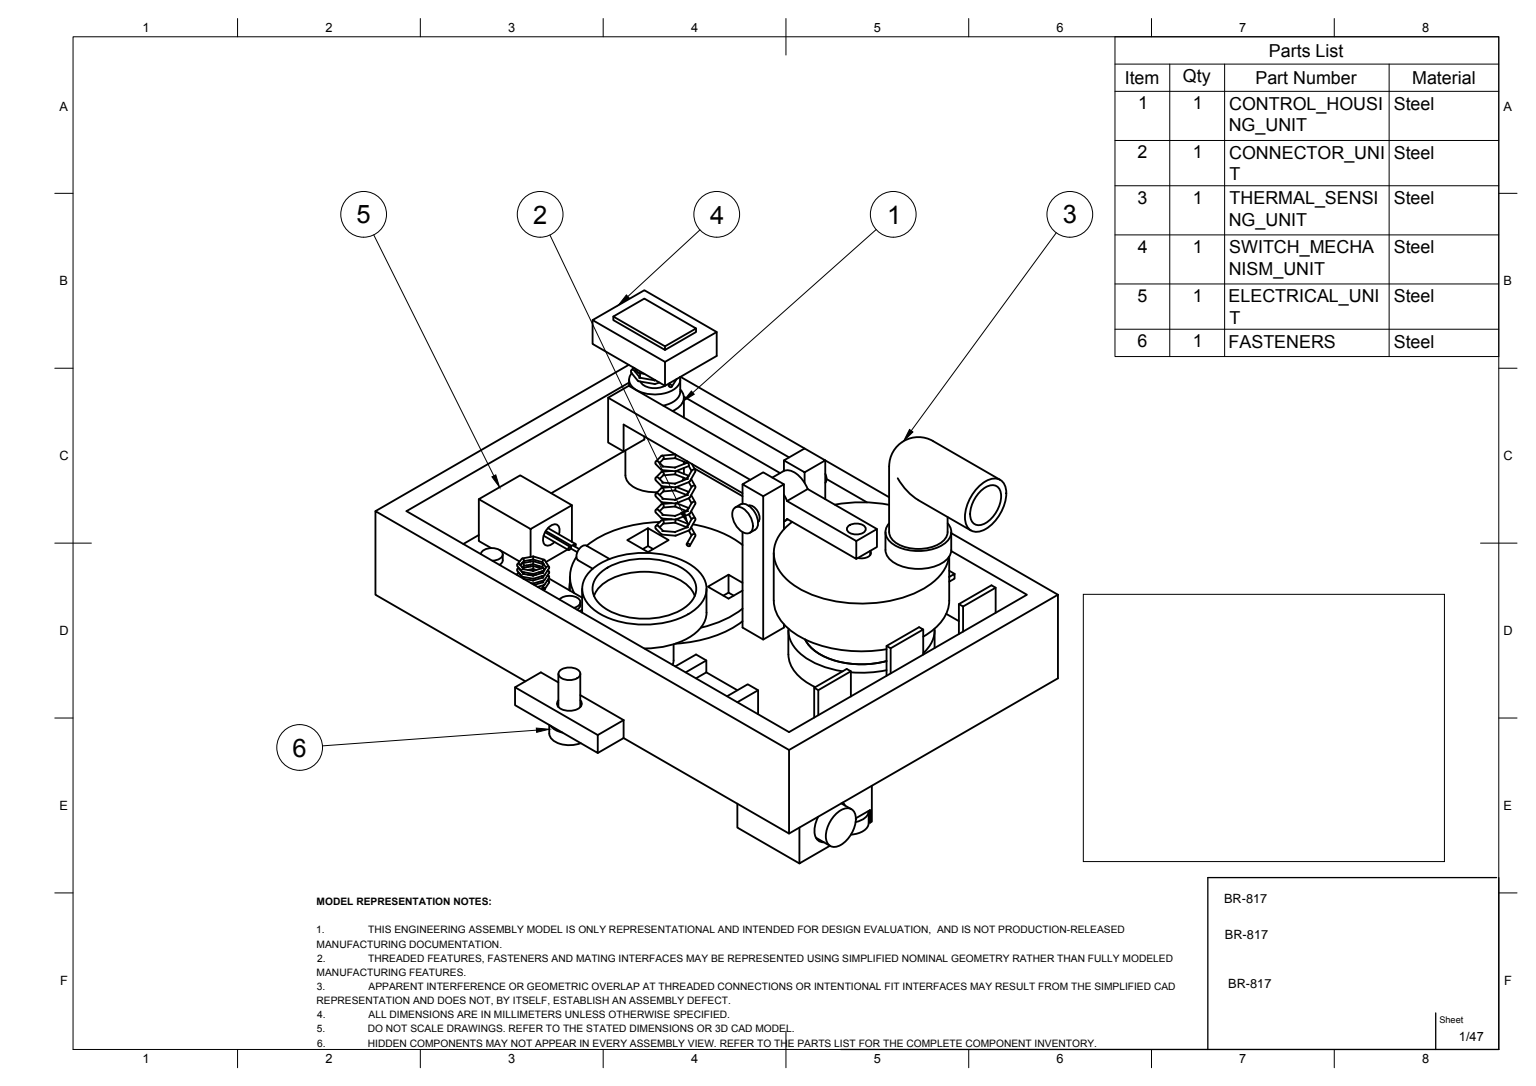
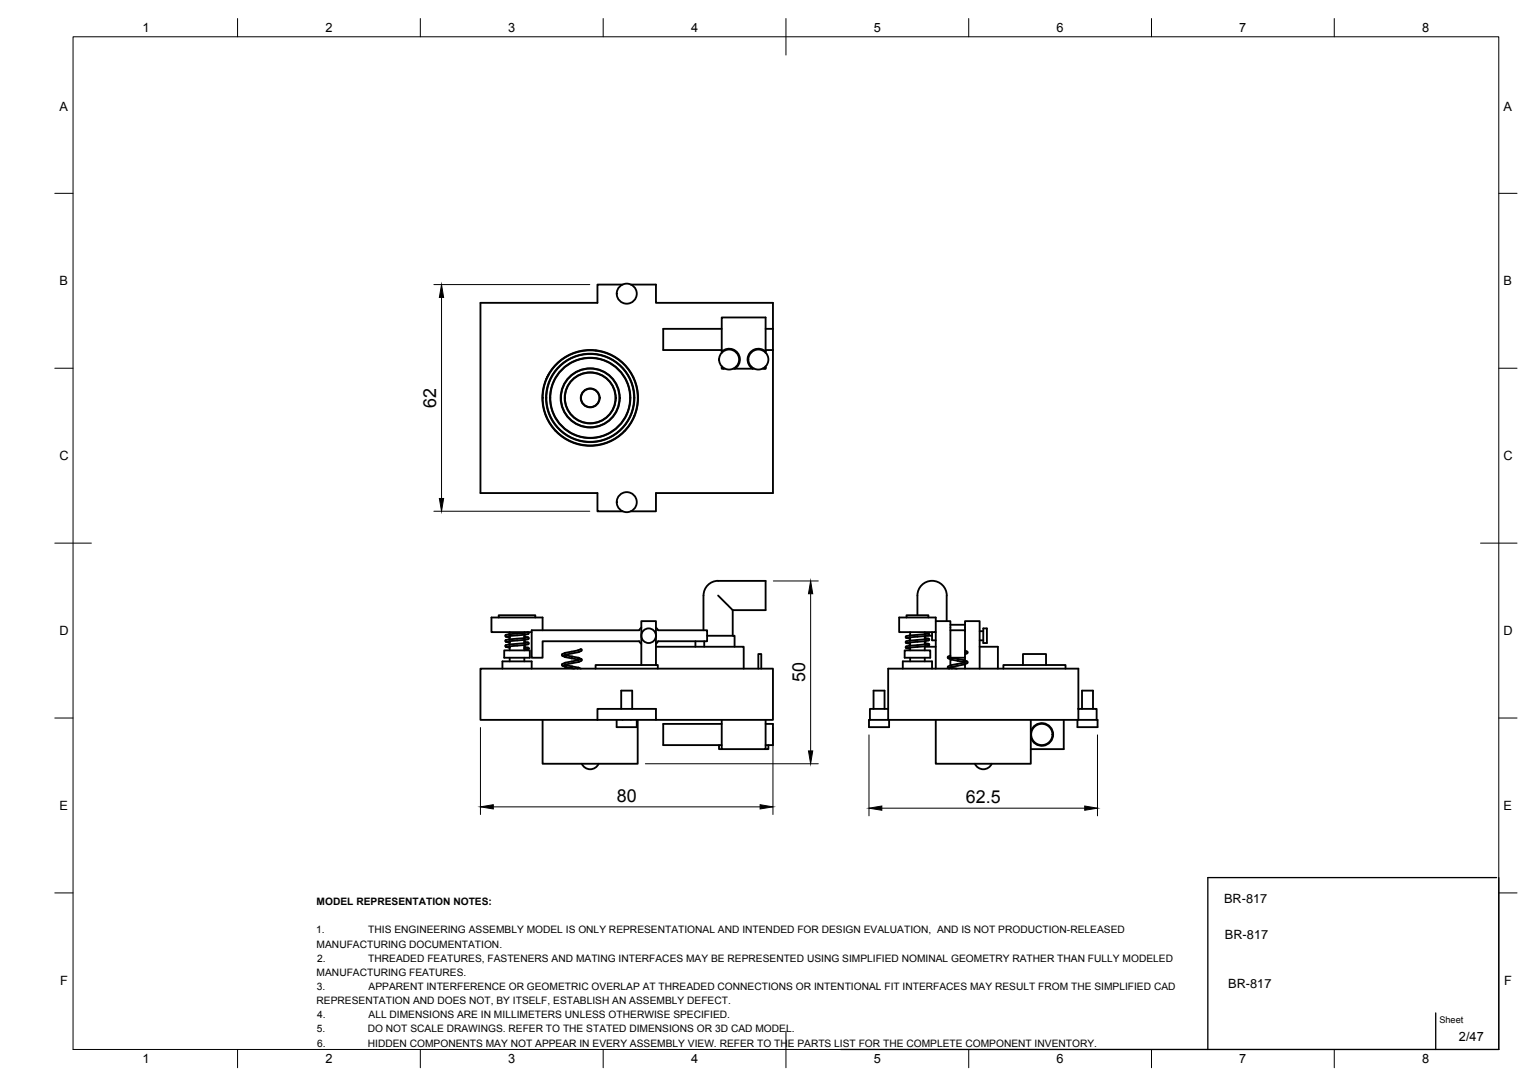
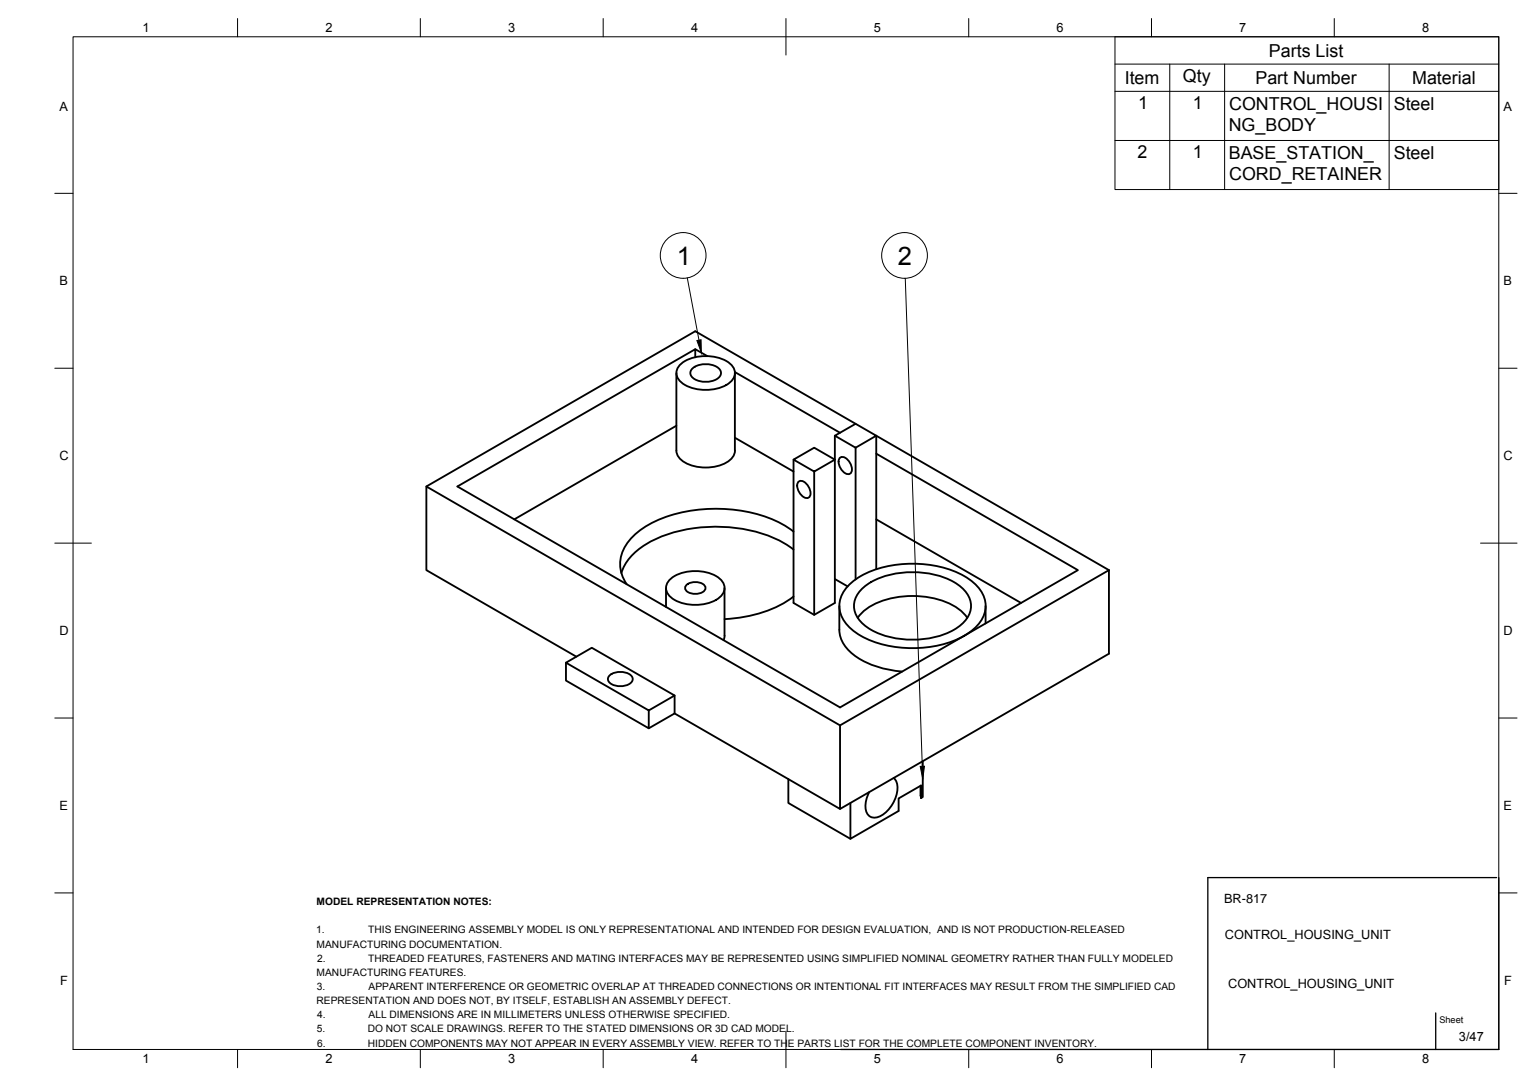
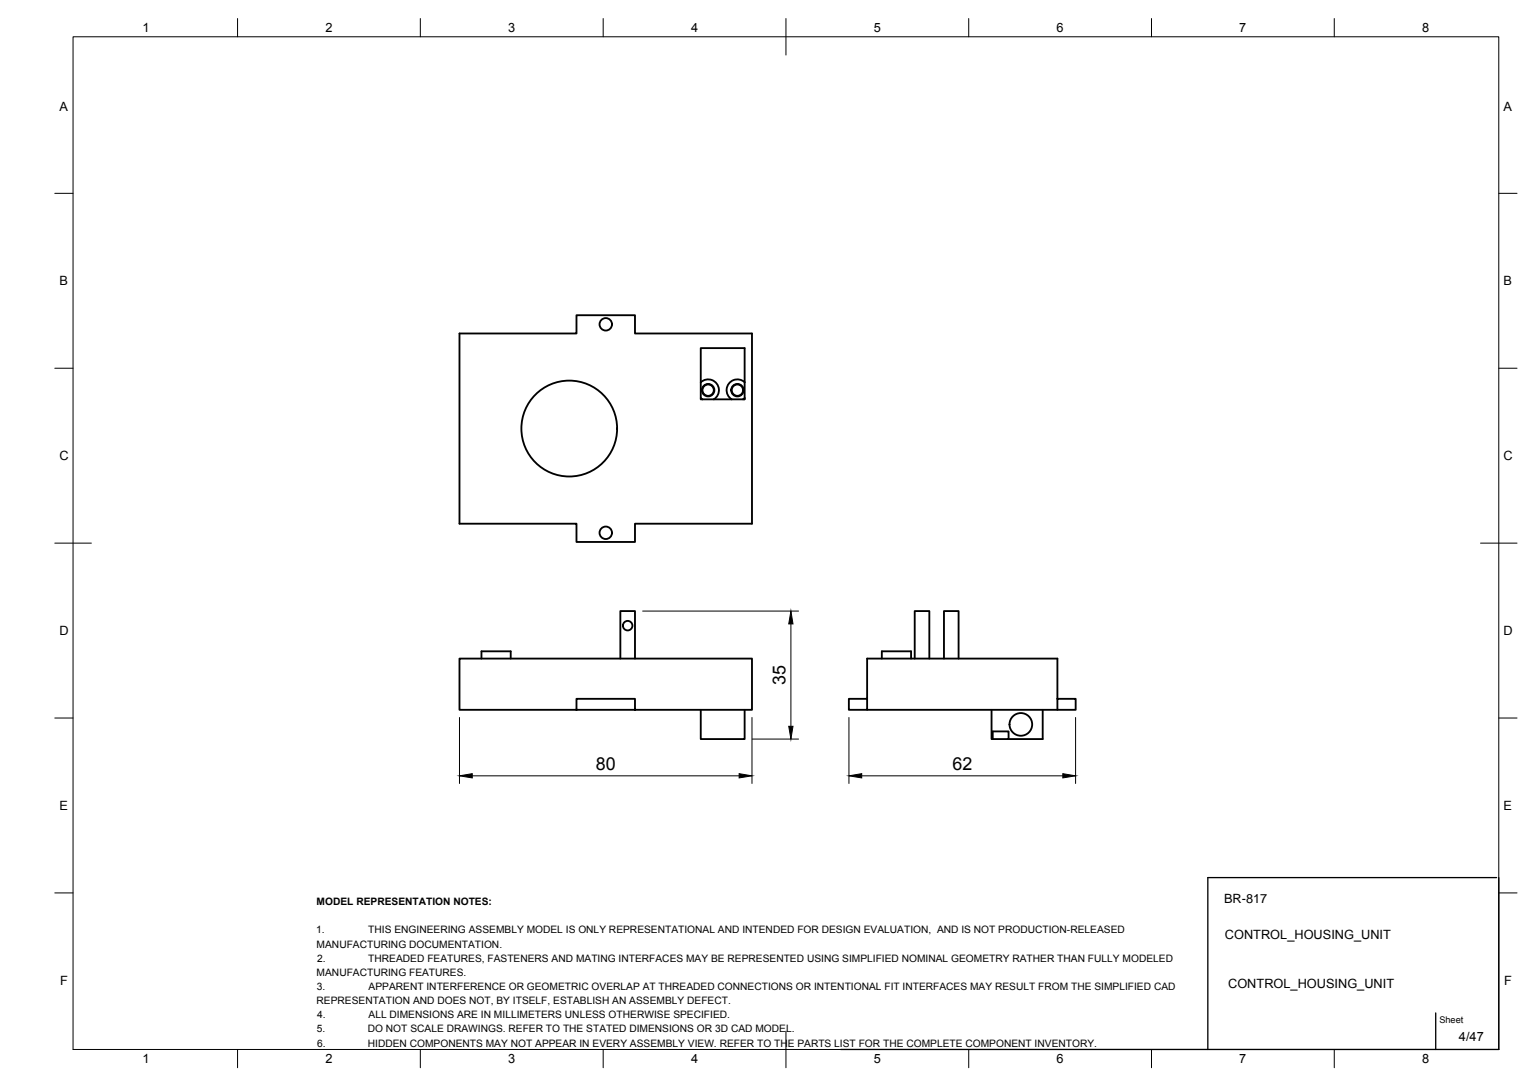
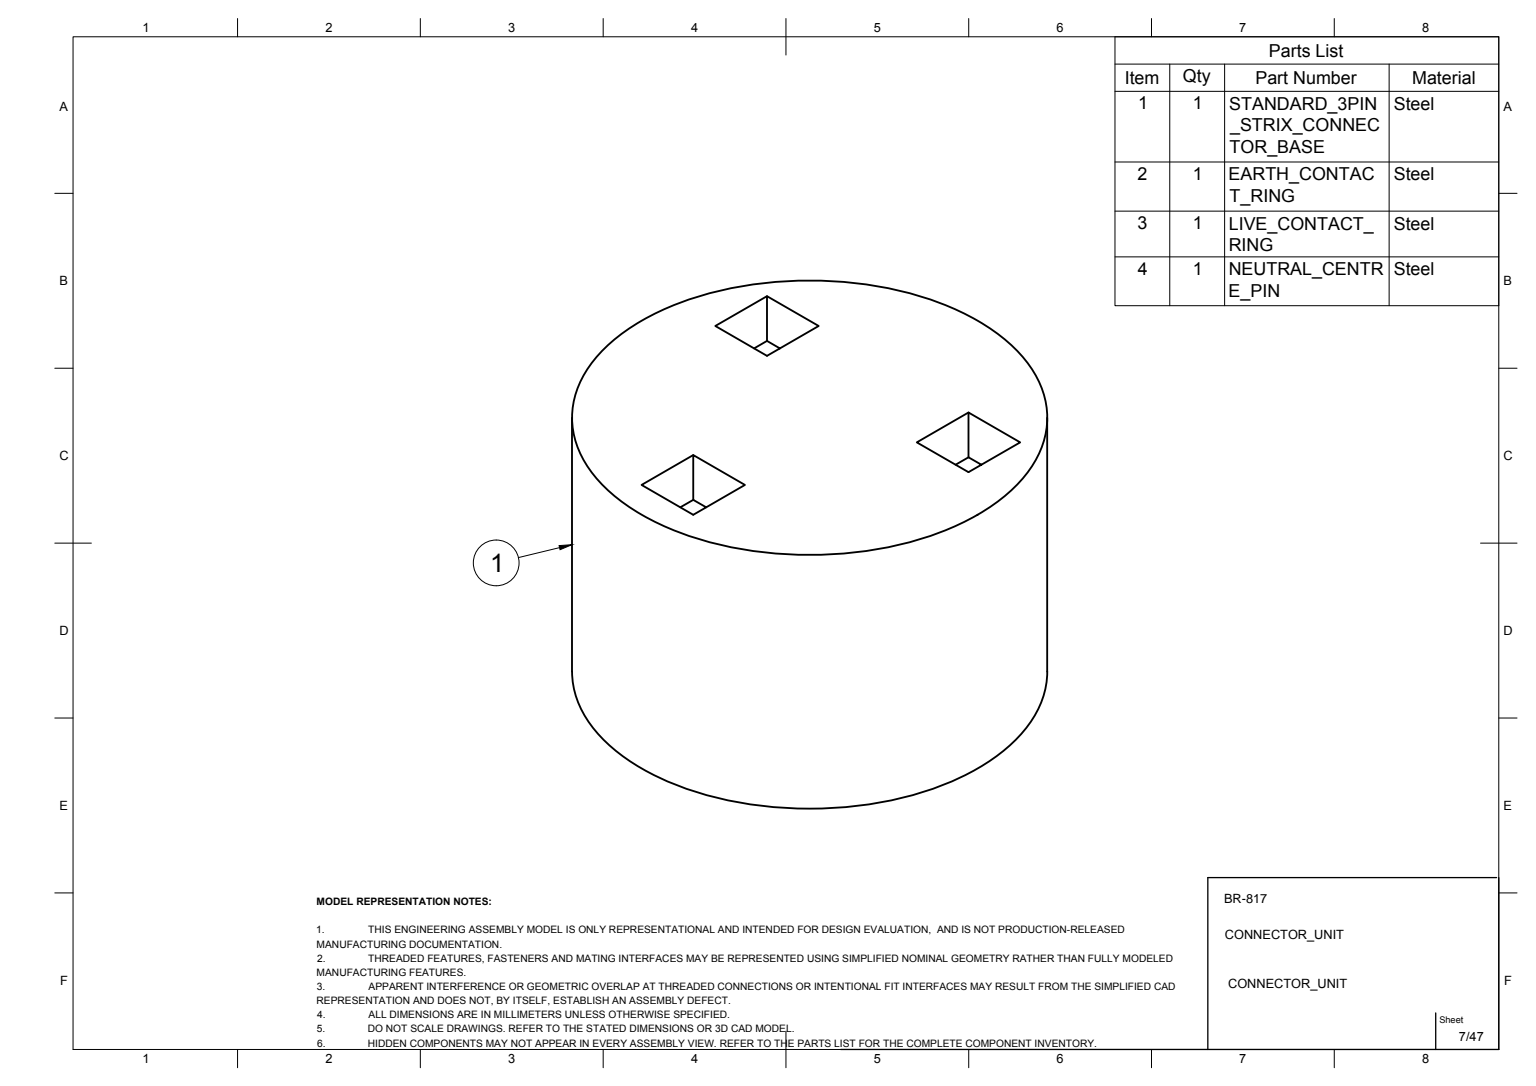
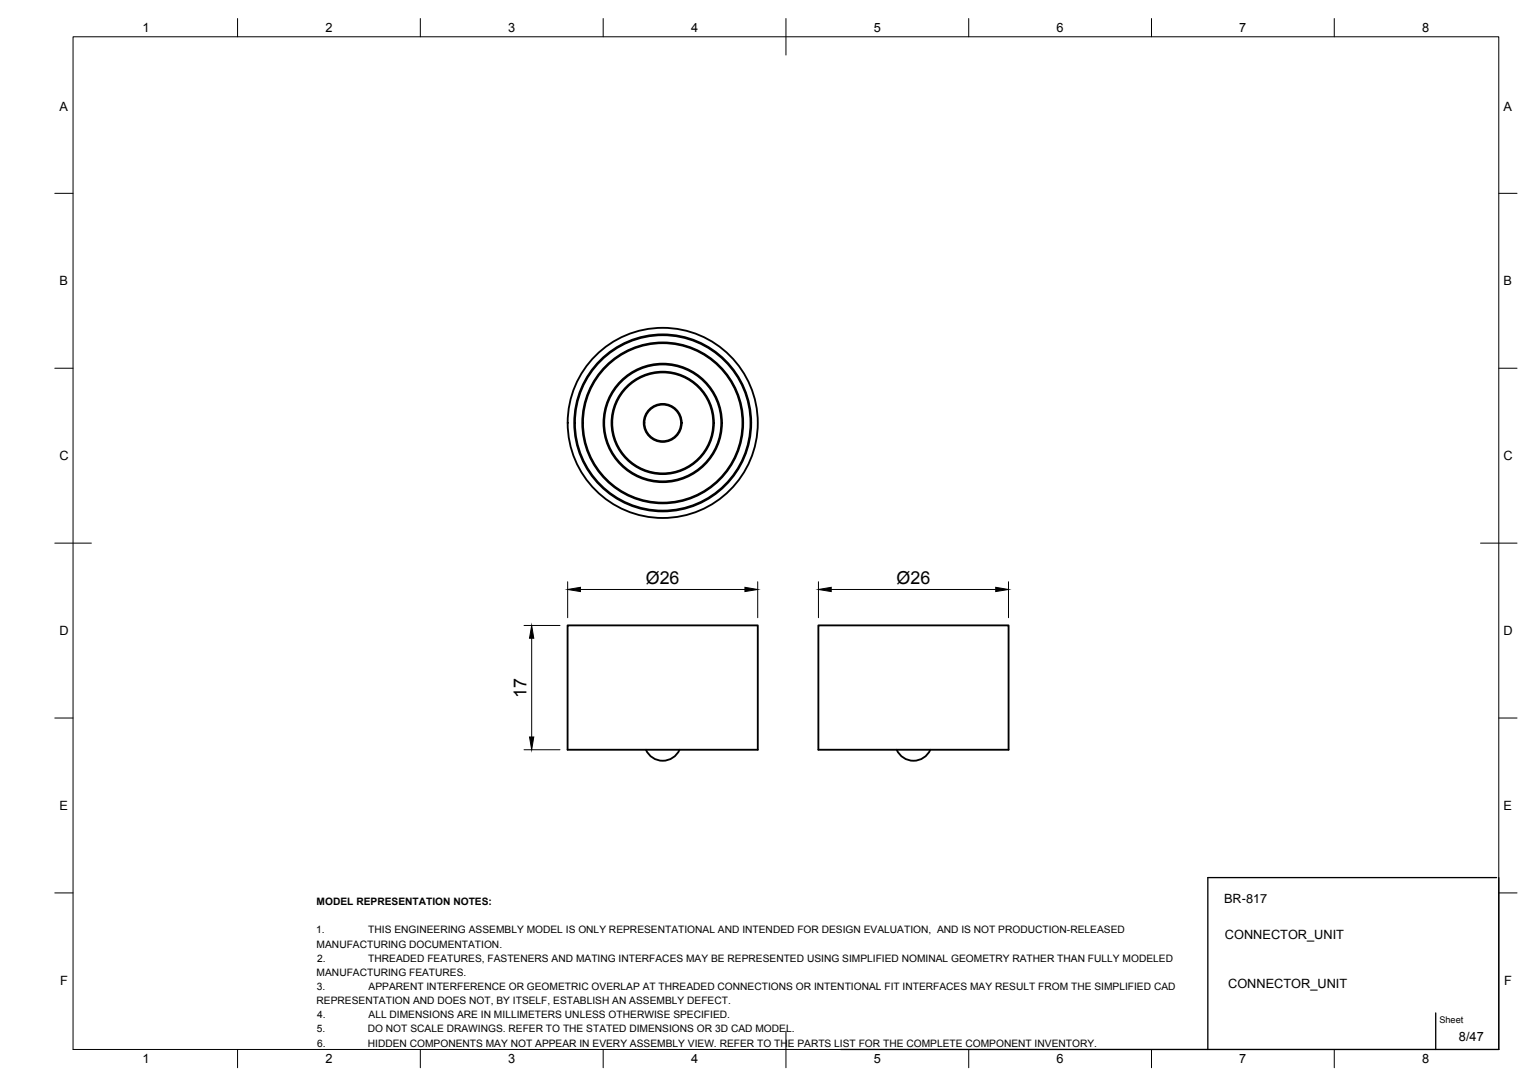
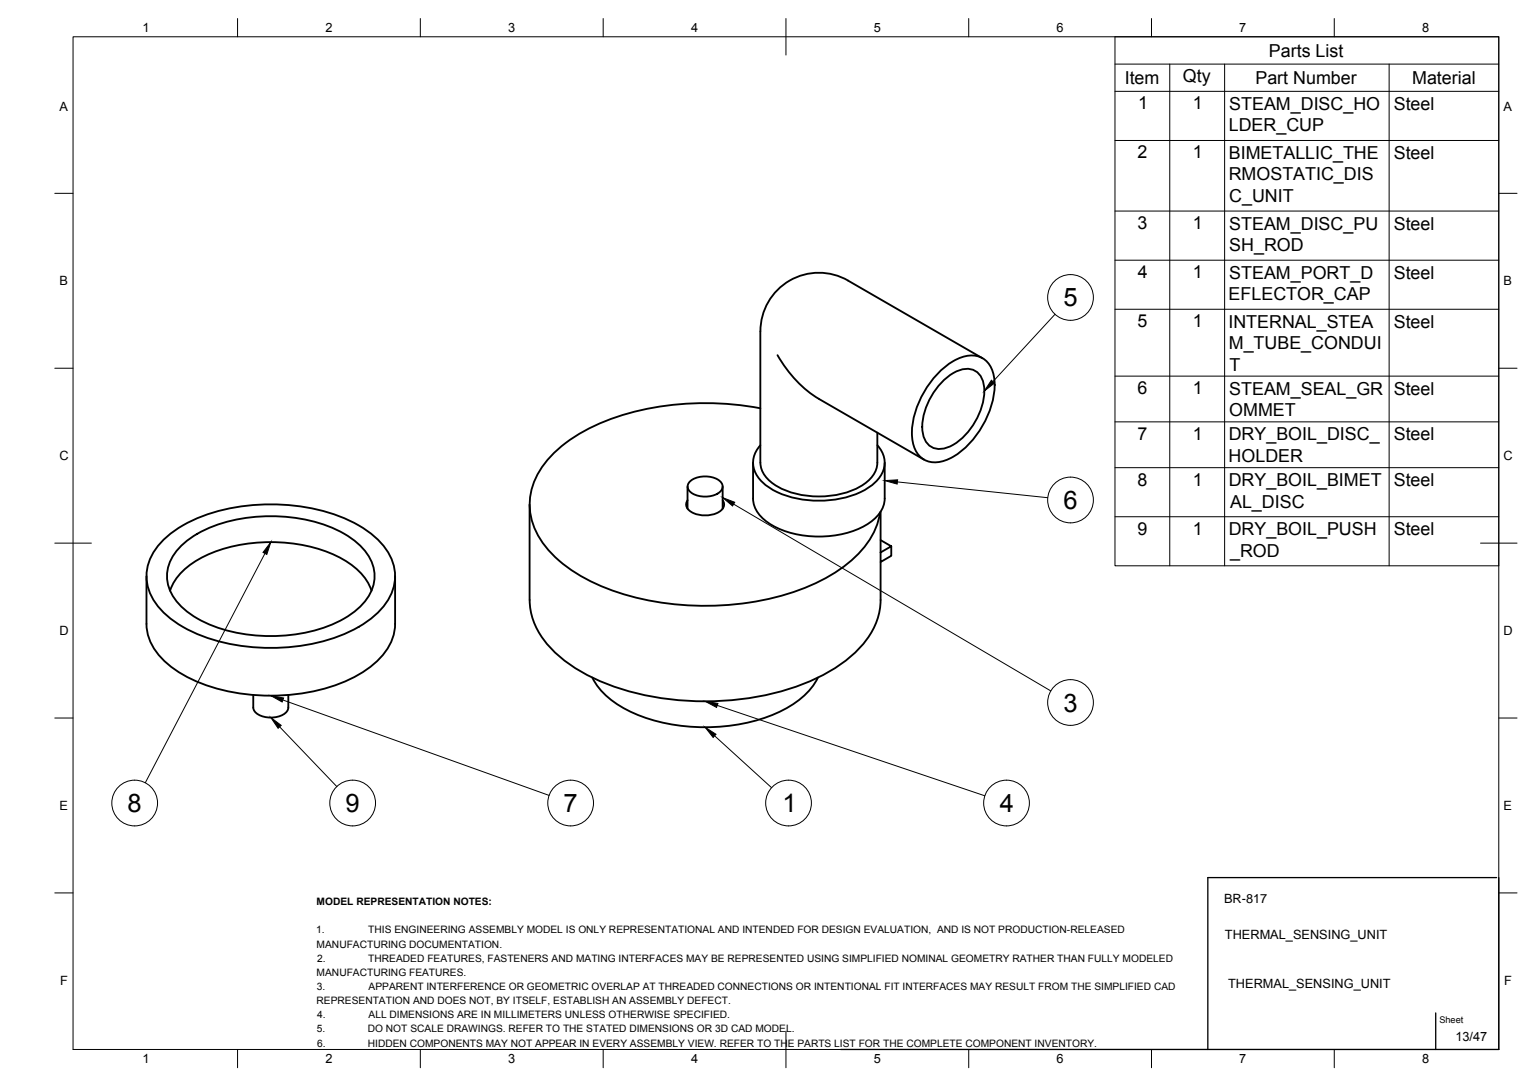
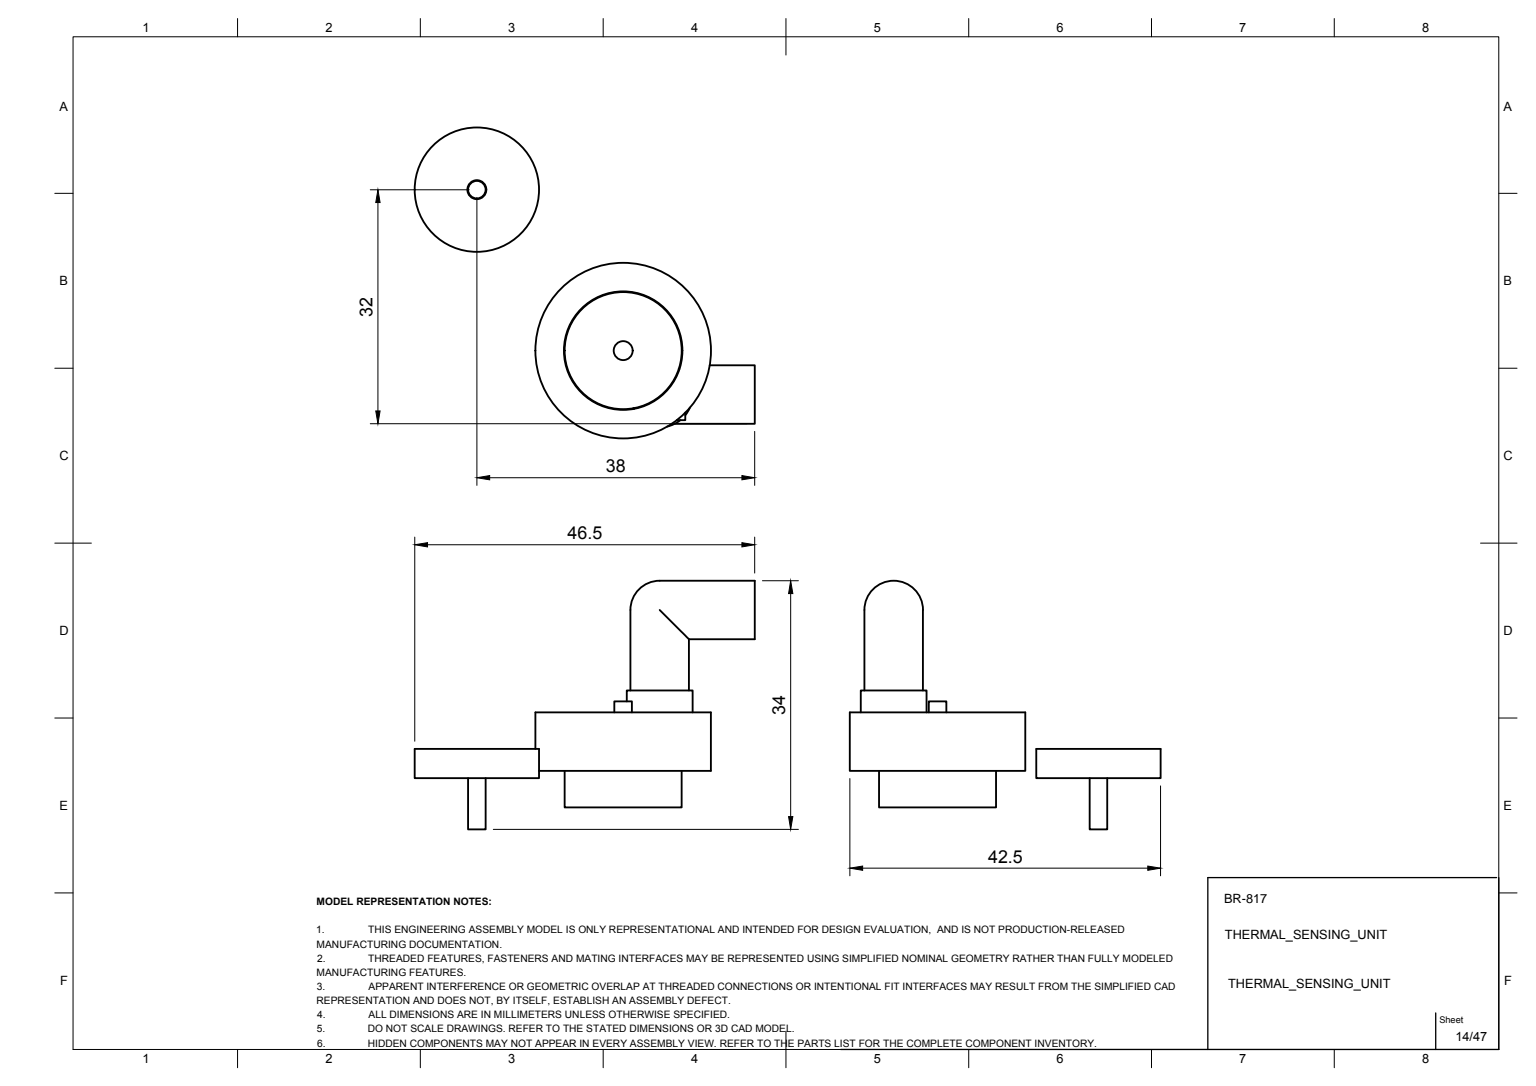
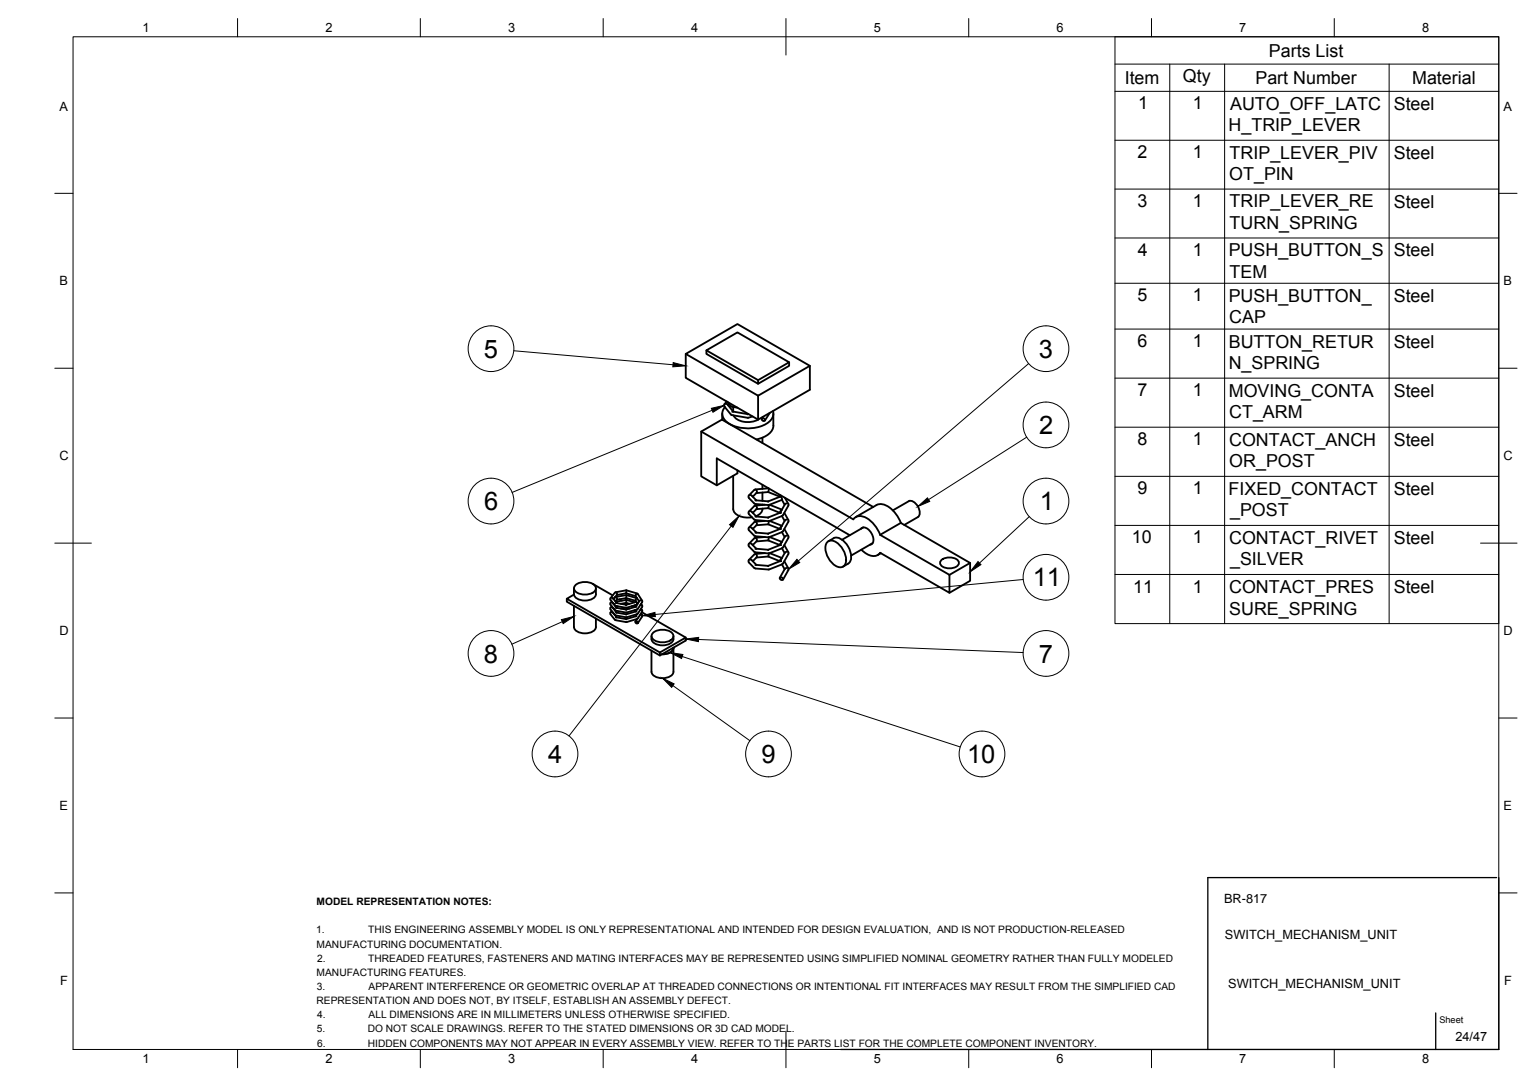
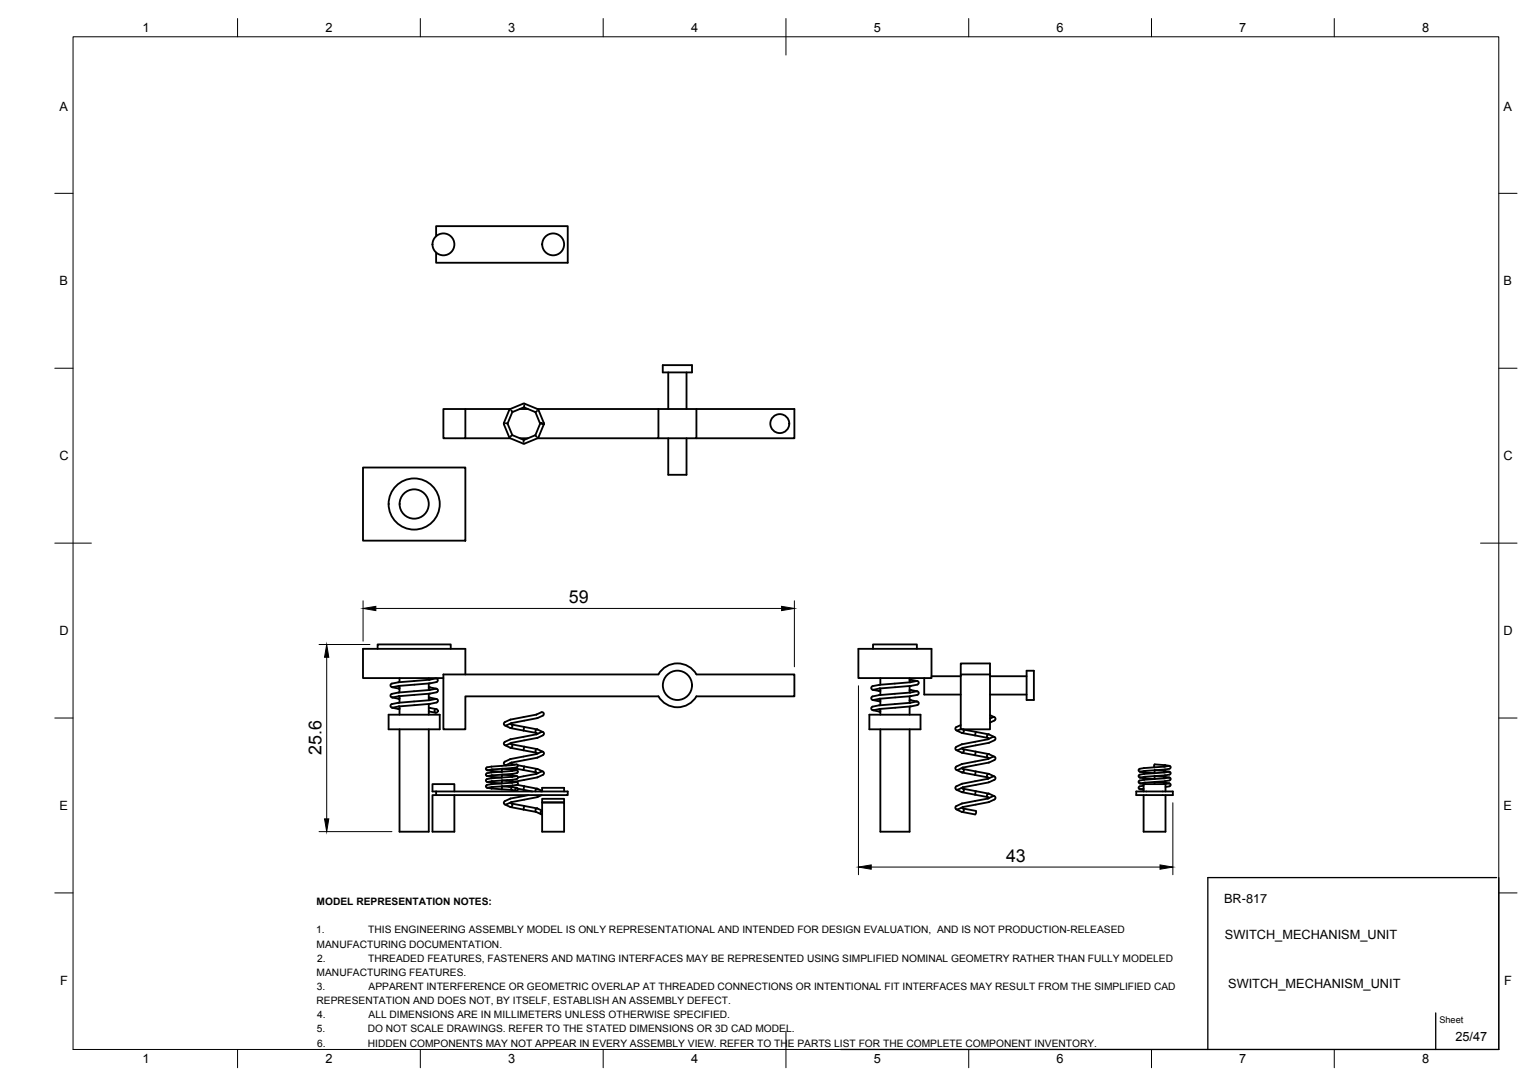
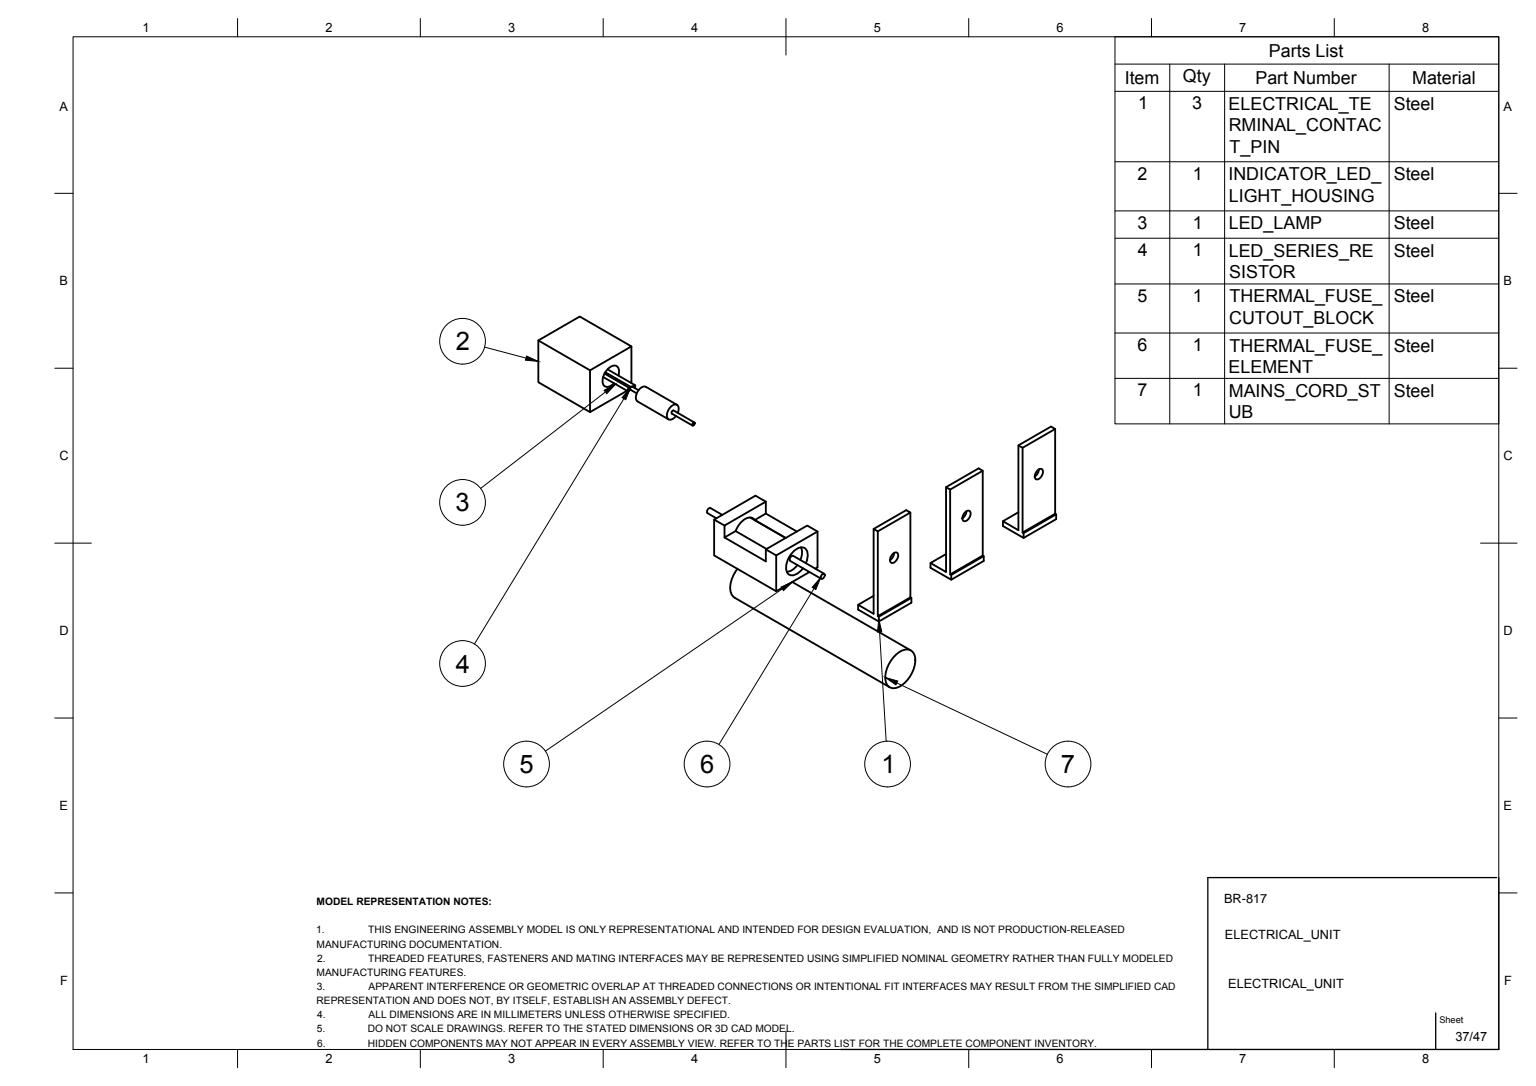
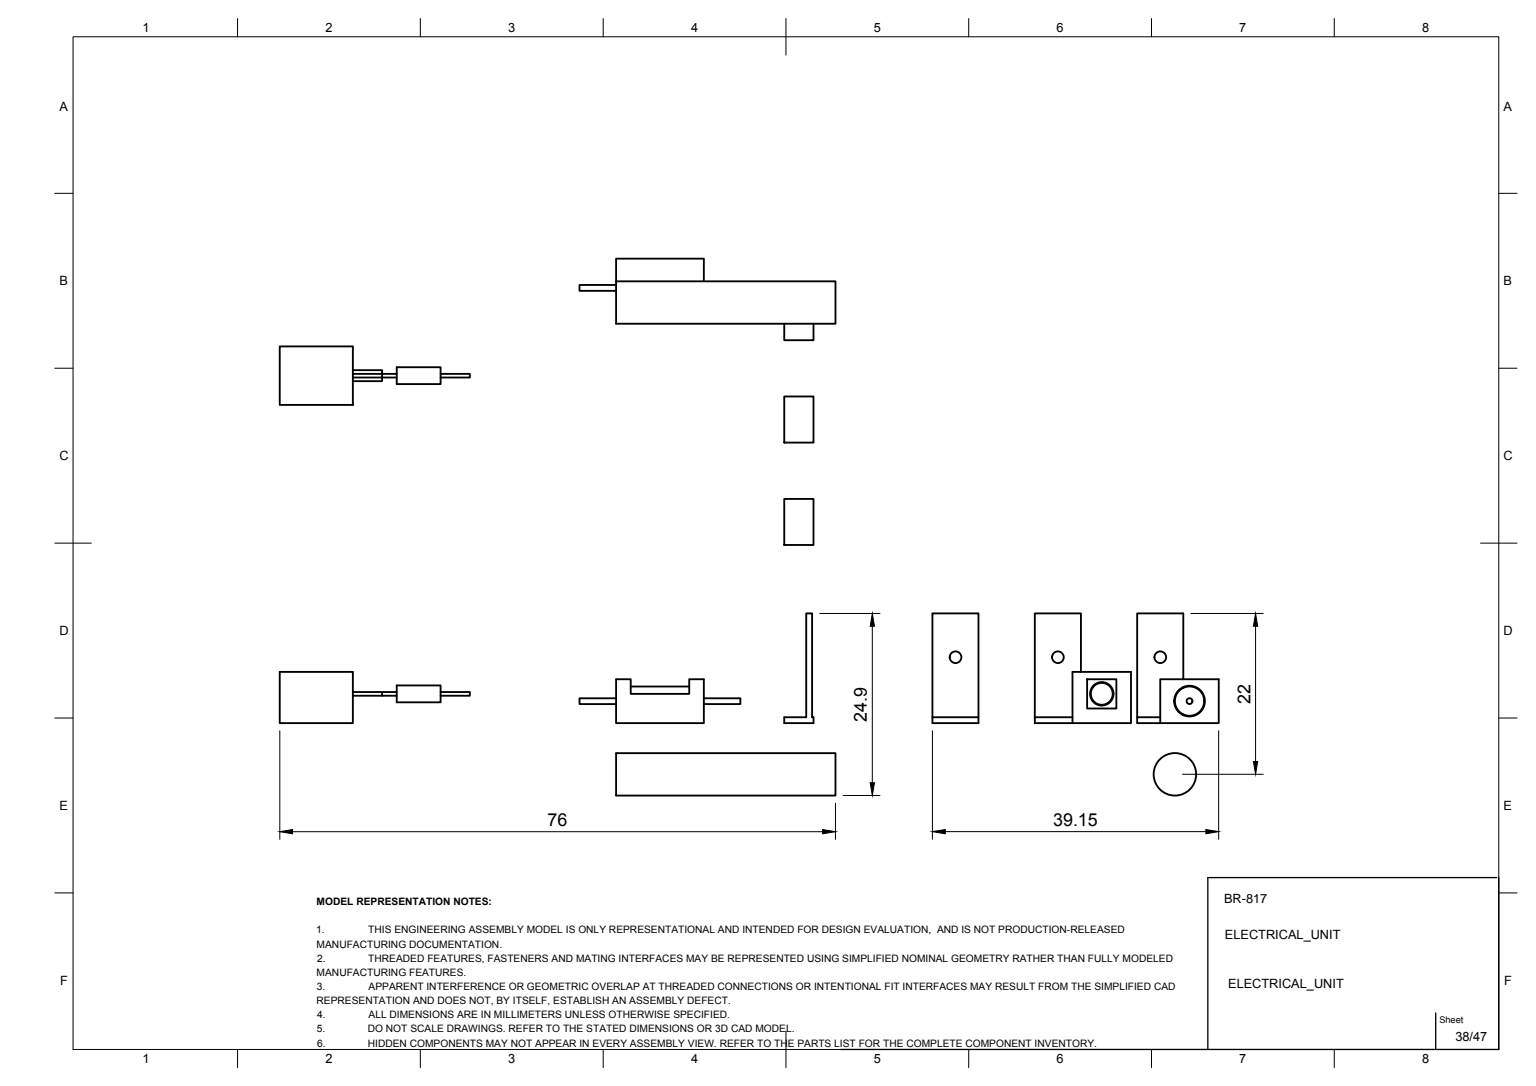
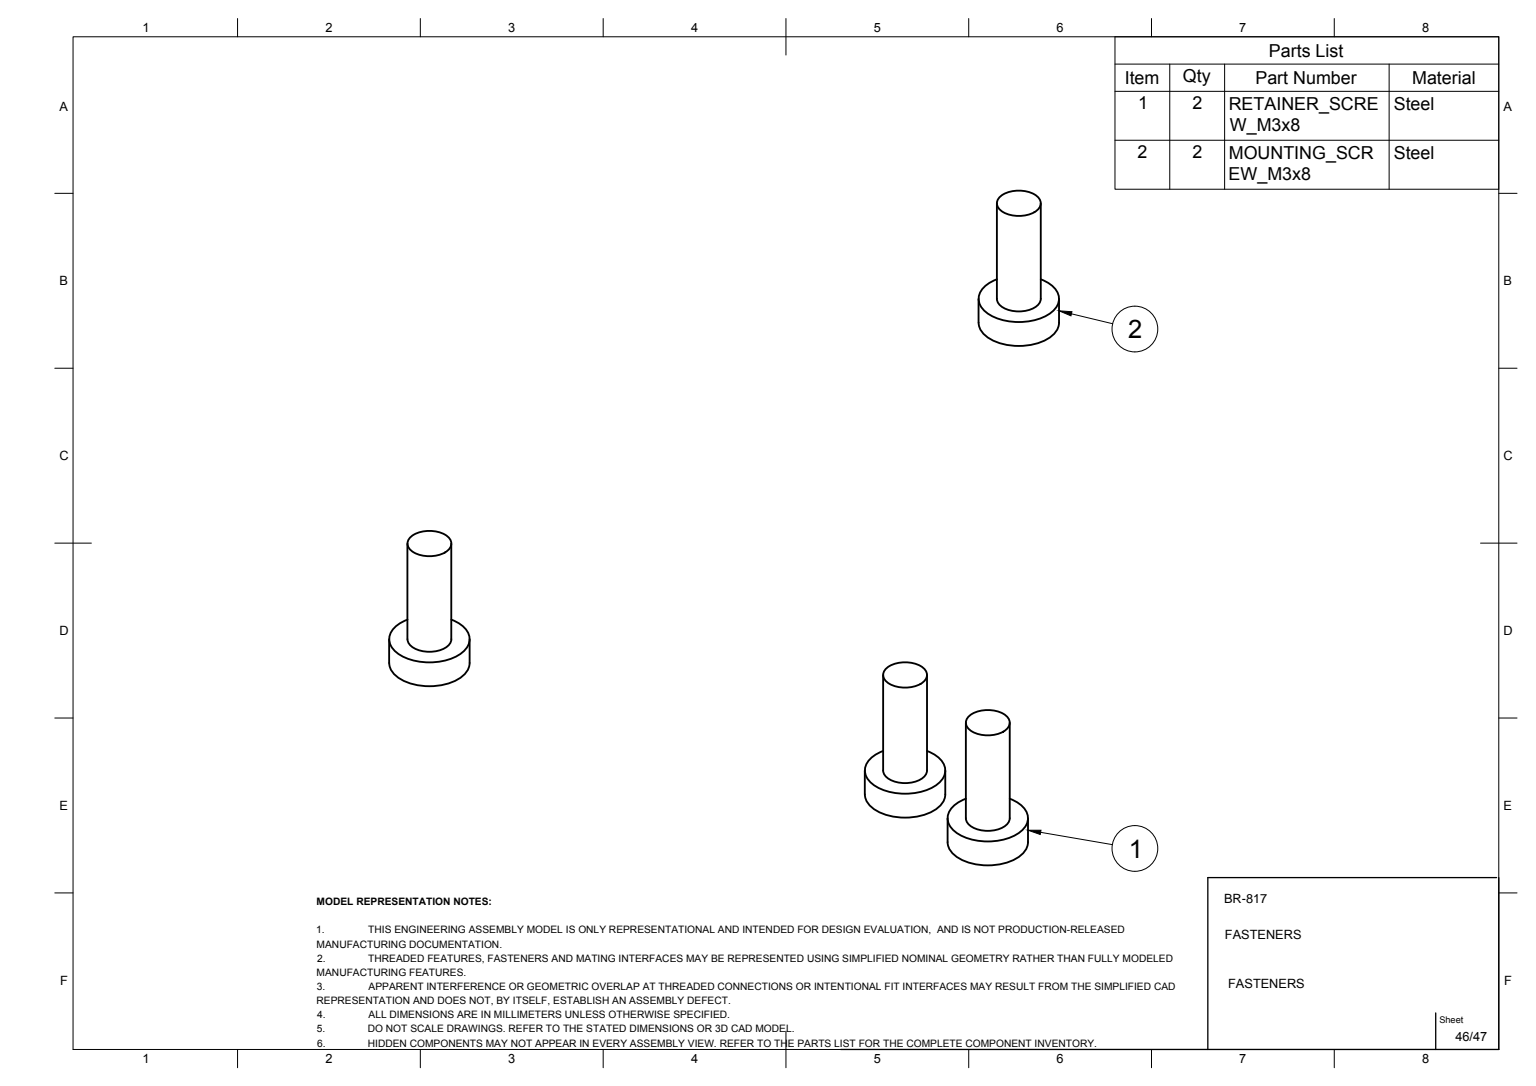
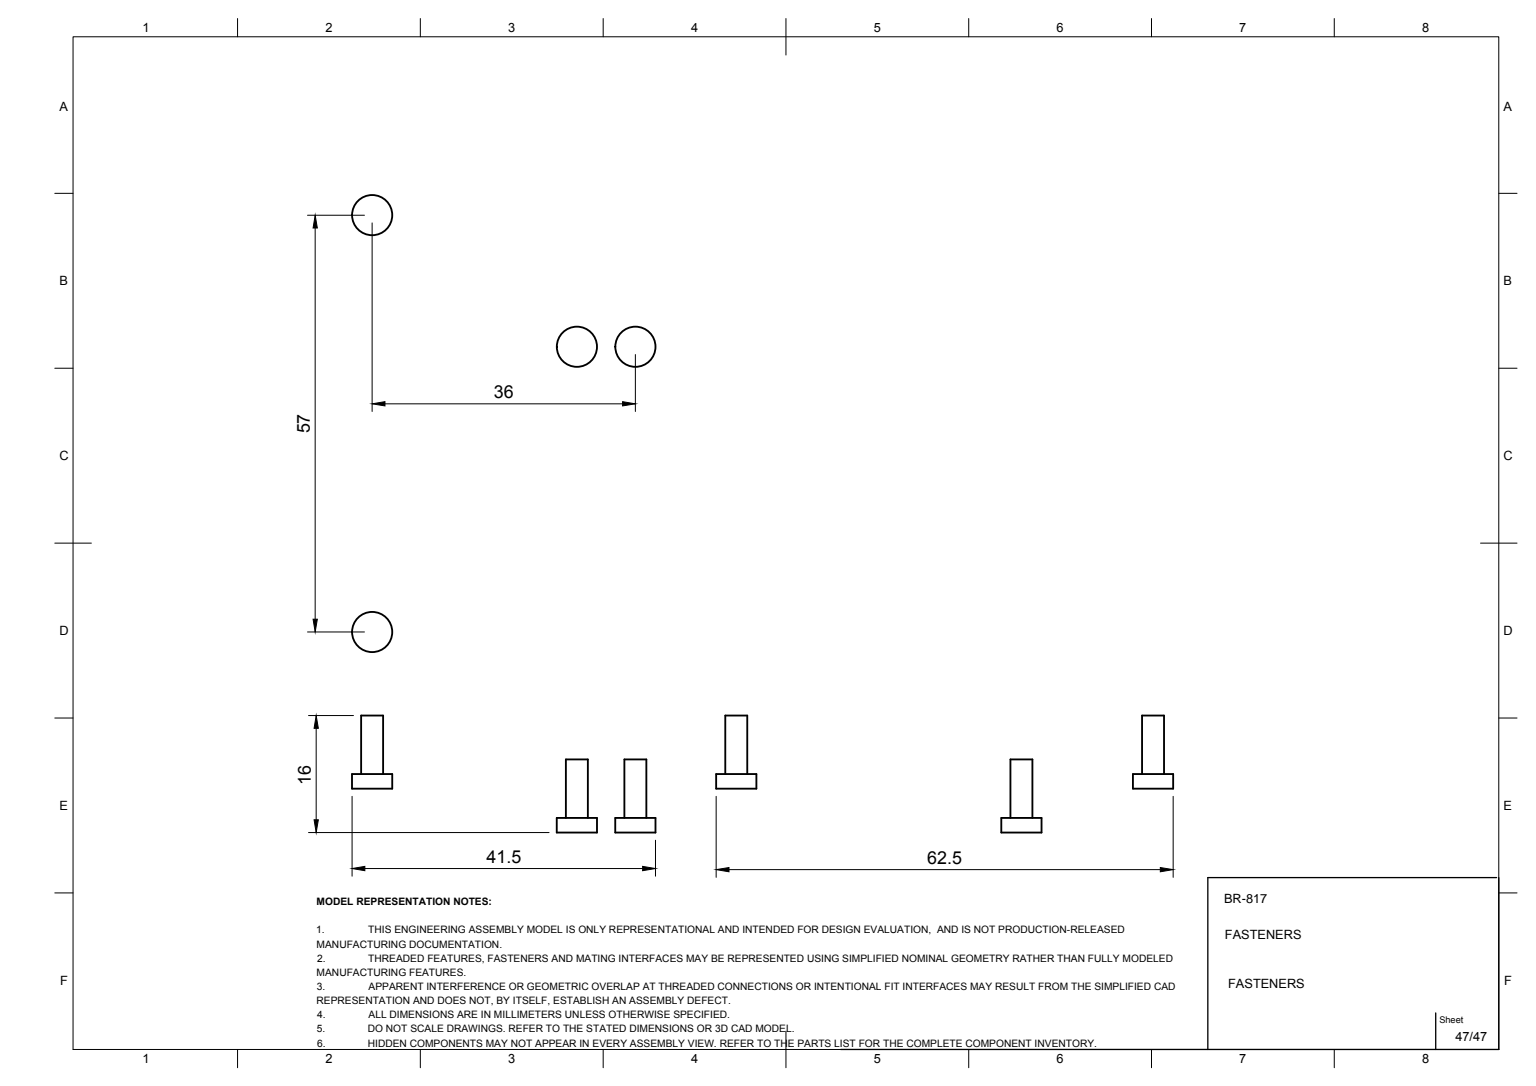
ISO-10303-21;
HEADER;
FILE_DESCRIPTION((''),'2;1');
FILE_NAME('BR-817','2026-10-01T22:07:29-07:00',(''),(''),'','','');
FILE_SCHEMA (('AUTOMOTIVE_DESIGN { 1 0 10303 214 3 1 1 }'));
ENDSEC;
DATA;
#10 = MECHANICAL_DESIGN_GEOMETRIC_PRESENTATION_REPRESENTATION('',(#543,#544,
#545,#546,#547,#548,#549,#550,#551,#552,#553,#554,#555,#556,#557,#558,#559,
#560,#561,#562,#563,#564,#565,#566,#567,#568,#569,#570,#571,#572,#573,#574,
#575,#576,#577,#578,#579,#580,#581,#582,#583,#584),#15484) ;
#11 = B_SPLINE_CURVE_WITH_KNOTS('',3,(#13547,#13548,#13549,#13550,#13551,
#13552,#13553,#13554,#13555,#13556,#13557,#13558,#13559,#13560,#13561,#13562,
#13563,#13564,#13565,#13566,#13567,#13568),.UNSPECIFIED.,.F.,.F.,(4,2,2,
2,2,2,2,2,2,2,4),(-0.956775615070491,-0.896341583425282,-0.835907551780074,
-0.715039488489657,-0.596713648012451,-0.478387807535245,-0.36006196705804,
-0.241736126580834,-0.120868063290417,-0.0604340316452086,0.),
 .UNSPECIFIED.) ;
#12 = B_SPLINE_CURVE_WITH_KNOTS('',3,(#13586,#13587,#13588,#13589,#13590,
#13591,#13592,#13593,#13594,#13595,#13596,#13597,#13598,#13599,#13600,#13601,
#13602,#13603,#13604,#13605,#13606,#13607),.UNSPECIFIED.,.F.,.F.,(4,2,2,
2,2,2,2,2,2,2,4),(0.,0.0604340316452085,0.120868063290417,0.241736126580834,
0.36006196705804,0.478387807535245,0.596713648012451,0.715039488489657,
0.835907551780074,0.896341583425282,0.956775615070491),.UNSPECIFIED.) ;
#13 = ELLIPSE('',#8939,0.424264068711929,0.3) ;
#14 = ELLIPSE('',#8947,0.565685424949238,0.4) ;
#15 = ELLIPSE('',#9204,0.0269900326446259,0.025) ;
#16 = ELLIPSE('',#9205,0.0269900326446259,0.025) ;
#17 = ELLIPSE('',#9206,0.0269900326446259,0.025) ;
#18 = ELLIPSE('',#9209,0.026990032644626,0.025) ;
#19 = ELLIPSE('',#9210,0.026990032644626,0.025) ;
#20 = ELLIPSE('',#9212,0.026990032644626,0.025) ;
#21 = ELLIPSE('',#9214,0.026990032644626,0.025) ;
#22 = ELLIPSE('',#9216,0.0269900326446258,0.025) ;
#23 = ELLIPSE('',#9218,0.0269900326446259,0.025) ;
#24 = ELLIPSE('',#9219,0.0269900326446259,0.025) ;
#25 = ELLIPSE('',#9221,0.026990032644626,0.025) ;
#26 = ELLIPSE('',#9222,0.026990032644626,0.025) ;
#27 = ELLIPSE('',#9223,0.026990032644626,0.025) ;
#28 = ELLIPSE('',#9225,0.026990032644626,0.025) ;
#29 = ELLIPSE('',#9226,0.026990032644626,0.025) ;
#30 = ELLIPSE('',#9228,0.0269900326446259,0.025) ;
#31 = ELLIPSE('',#9229,0.0269900326446259,0.025) ;
#32 = ELLIPSE('',#9230,0.0269900326446259,0.025) ;
#33 = ELLIPSE('',#9232,0.026990032644626,0.025) ;
#34 = ELLIPSE('',#9233,0.026990032644626,0.025) ;
#35 = ELLIPSE('',#9235,0.0269900326446259,0.025) ;
#36 = ELLIPSE('',#9237,0.026990032644626,0.025) ;
#37 = ELLIPSE('',#9239,0.026990032644626,0.025) ;
#38 = ELLIPSE('',#9241,0.0269900326446259,0.025) ;
#39 = ELLIPSE('',#9242,0.0269900326446259,0.025) ;
#40 = ELLIPSE('',#9244,0.026990032644626,0.025) ;
#41 = ELLIPSE('',#9245,0.026990032644626,0.025) ;
#42 = ELLIPSE('',#9246,0.026990032644626,0.025) ;
#43 = ELLIPSE('',#9248,0.0269900326446259,0.025) ;
#44 = ELLIPSE('',#9249,0.0269900326446259,0.025) ;
#45 = ELLIPSE('',#9251,0.0269900326446258,0.025) ;
#46 = ELLIPSE('',#9252,0.0269900326446258,0.025) ;
#47 = ELLIPSE('',#9253,0.0269900326446258,0.025) ;
#48 = ELLIPSE('',#9255,0.0269900326446259,0.025) ;
#49 = ELLIPSE('',#9256,0.0269900326446259,0.025) ;
#50 = ELLIPSE('',#9258,0.0269900326446259,0.025) ;
#51 = ELLIPSE('',#9260,0.026990032644626,0.025) ;
#52 = ELLIPSE('',#9262,0.0269900326446259,0.025) ;
#53 = ELLIPSE('',#9264,0.026990032644626,0.025) ;
#54 = ELLIPSE('',#9265,0.026990032644626,0.025) ;
#55 = ELLIPSE('',#9267,0.026990032644626,0.025) ;
#56 = ELLIPSE('',#9268,0.026990032644626,0.025) ;
#57 = ELLIPSE('',#9269,0.026990032644626,0.025) ;
#58 = ELLIPSE('',#9271,0.026990032644626,0.025) ;
#59 = ELLIPSE('',#9272,0.026990032644626,0.025) ;
#60 = ELLIPSE('',#9274,0.0269900326446259,0.025) ;
#61 = ELLIPSE('',#9275,0.0269900326446259,0.025) ;
#62 = ELLIPSE('',#9276,0.0269900326446259,0.025) ;
#63 = ELLIPSE('',#9278,0.0269900326446259,0.025) ;
#64 = ELLIPSE('',#9279,0.0269900326446259,0.025) ;
#65 = ELLIPSE('',#9281,0.0269900326446259,0.025) ;
#66 = ELLIPSE('',#9283,0.026990032644626,0.025) ;
#67 = ELLIPSE('',#9285,0.0269900326446259,0.025) ;
#68 = ELLIPSE('',#9287,0.0269900326446259,0.025) ;
#69 = ELLIPSE('',#9288,0.0269900326446259,0.025) ;
#70 = ELLIPSE('',#9290,0.026990032644626,0.025) ;
#71 = ELLIPSE('',#9291,0.026990032644626,0.025) ;
#72 = ELLIPSE('',#9292,0.026990032644626,0.025) ;
#73 = ELLIPSE('',#9294,0.0269900326446259,0.025) ;
#74 = ELLIPSE('',#9295,0.0269900326446259,0.025) ;
#75 = ELLIPSE('',#9297,0.0269900326446259,0.025) ;
#76 = ELLIPSE('',#9298,0.0269900326446259,0.025) ;
#77 = ELLIPSE('',#9299,0.0269900326446259,0.025) ;
#78 = ELLIPSE('',#9301,0.0269900326446259,0.025) ;
#79 = ELLIPSE('',#9302,0.0269900326446259,0.025) ;
#80 = ELLIPSE('',#9304,0.0269900326446259,0.025) ;
#81 = ELLIPSE('',#9306,0.026990032644626,0.025) ;
#82 = ELLIPSE('',#9308,0.0269900326446259,0.025) ;
#83 = ELLIPSE('',#9310,0.026990032644626,0.025) ;
#84 = ELLIPSE('',#9311,0.026990032644626,0.025) ;
#85 = ELLIPSE('',#9313,0.026990032644626,0.025) ;
#86 = ELLIPSE('',#9314,0.026990032644626,0.025) ;
#87 = ELLIPSE('',#9315,0.026990032644626,0.025) ;
#88 = ELLIPSE('',#9445,0.0270464082562617,0.025) ;
#89 = ELLIPSE('',#9446,0.0270464082562617,0.025) ;
#90 = ELLIPSE('',#9447,0.0270464082562617,0.025) ;
#91 = ELLIPSE('',#9450,0.0270464082562613,0.025) ;
#92 = ELLIPSE('',#9451,0.0270464082562613,0.025) ;
#93 = ELLIPSE('',#9453,0.0270464082562612,0.025) ;
#94 = ELLIPSE('',#9455,0.0270464082562616,0.025) ;
#95 = ELLIPSE('',#9457,0.0270464082562615,0.025) ;
#96 = ELLIPSE('',#9459,0.0270464082562615,0.025) ;
#97 = ELLIPSE('',#9460,0.0270464082562615,0.025) ;
#98 = ELLIPSE('',#9462,0.0270464082562615,0.025) ;
#99 = ELLIPSE('',#9463,0.0270464082562615,0.025) ;
#100 = ELLIPSE('',#9464,0.0270464082562615,0.025) ;
#101 = ELLIPSE('',#9466,0.0270464082562616,0.025) ;
#102 = ELLIPSE('',#9467,0.0270464082562616,0.025) ;
#103 = ELLIPSE('',#9469,0.0270464082562617,0.025) ;
#104 = ELLIPSE('',#9470,0.0270464082562617,0.025) ;
#105 = ELLIPSE('',#9471,0.0270464082562617,0.025) ;
#106 = ELLIPSE('',#9473,0.0270464082562615,0.025) ;
#107 = ELLIPSE('',#9474,0.0270464082562615,0.025) ;
#108 = ELLIPSE('',#9476,0.0270464082562614,0.025) ;
#109 = ELLIPSE('',#9478,0.0270464082562616,0.025) ;
#110 = ELLIPSE('',#9480,0.0270464082562617,0.025) ;
#111 = ELLIPSE('',#9482,0.0270464082562615,0.025) ;
#112 = ELLIPSE('',#9483,0.0270464082562615,0.025) ;
#113 = ELLIPSE('',#9485,0.0270464082562615,0.025) ;
#114 = ELLIPSE('',#9486,0.0270464082562615,0.025) ;
#115 = ELLIPSE('',#9487,0.0270464082562615,0.025) ;
#116 = ELLIPSE('',#9489,0.0270464082562617,0.025) ;
#117 = ELLIPSE('',#9490,0.0270464082562617,0.025) ;
#118 = ELLIPSE('',#9492,0.0270464082562616,0.025) ;
#119 = ELLIPSE('',#9493,0.0270464082562616,0.025) ;
#120 = ELLIPSE('',#9494,0.0270464082562616,0.025) ;
#121 = ELLIPSE('',#9496,0.0270464082562616,0.025) ;
#122 = ELLIPSE('',#9497,0.0270464082562616,0.025) ;
#123 = ELLIPSE('',#9499,0.0270464082562614,0.025) ;
#124 = ELLIPSE('',#9501,0.0270464082562616,0.025) ;
#125 = ELLIPSE('',#9503,0.0270464082562616,0.025) ;
#126 = ELLIPSE('',#9505,0.0270464082562616,0.025) ;
#127 = ELLIPSE('',#9506,0.0270464082562616,0.025) ;
#128 = ELLIPSE('',#9508,0.0270464082562615,0.025) ;
#129 = ELLIPSE('',#9509,0.0270464082562615,0.025) ;
#130 = ELLIPSE('',#9510,0.0270464082562615,0.025) ;
#131 = ELLIPSE('',#9676,0.0216399563664951,0.02) ;
#132 = ELLIPSE('',#9677,0.0216399563664951,0.02) ;
#133 = ELLIPSE('',#9678,0.0216399563664951,0.02) ;
#134 = ELLIPSE('',#9681,0.0216399563664949,0.02) ;
#135 = ELLIPSE('',#9682,0.0216399563664949,0.02) ;
#136 = ELLIPSE('',#9684,0.0216399563664949,0.02) ;
#137 = ELLIPSE('',#9686,0.0216399563664949,0.02) ;
#138 = ELLIPSE('',#9688,0.021639956366495,0.02) ;
#139 = ELLIPSE('',#9690,0.021639956366495,0.02) ;
#140 = ELLIPSE('',#9691,0.021639956366495,0.02) ;
#141 = ELLIPSE('',#9693,0.0216399563664949,0.02) ;
#142 = ELLIPSE('',#9694,0.0216399563664949,0.02) ;
#143 = ELLIPSE('',#9695,0.0216399563664949,0.02) ;
#144 = ELLIPSE('',#9697,0.021639956366495,0.02) ;
#145 = ELLIPSE('',#9698,0.021639956366495,0.02) ;
#146 = ELLIPSE('',#9700,0.0216399563664951,0.02) ;
#147 = ELLIPSE('',#9701,0.0216399563664951,0.02) ;
#148 = ELLIPSE('',#9702,0.0216399563664951,0.02) ;
#149 = ELLIPSE('',#9704,0.0216399563664949,0.02) ;
#150 = ELLIPSE('',#9705,0.0216399563664949,0.02) ;
#151 = ELLIPSE('',#9707,0.0216399563664949,0.02) ;
#152 = ELLIPSE('',#9709,0.021639956366495,0.02) ;
#153 = ELLIPSE('',#9711,0.0216399563664949,0.02) ;
#154 = ELLIPSE('',#9713,0.021639956366495,0.02) ;
#155 = ELLIPSE('',#9714,0.021639956366495,0.02) ;
#156 = ELLIPSE('',#9716,0.021639956366495,0.02) ;
#157 = ELLIPSE('',#9717,0.021639956366495,0.02) ;
#158 = ELLIPSE('',#9718,0.021639956366495,0.02) ;
#159 = ELLIPSE('',#9720,0.021639956366495,0.02) ;
#160 = ELLIPSE('',#9721,0.021639956366495,0.02) ;
#161 = ELLIPSE('',#9723,0.021639956366495,0.02) ;
#162 = ELLIPSE('',#9724,0.021639956366495,0.02) ;
#163 = ELLIPSE('',#9725,0.021639956366495,0.02) ;
#164 = ELLIPSE('',#9727,0.021639956366495,0.02) ;
#165 = ELLIPSE('',#9728,0.021639956366495,0.02) ;
#166 = ELLIPSE('',#9730,0.0216399563664949,0.02) ;
#167 = ELLIPSE('',#9732,0.021639956366495,0.02) ;
#168 = ELLIPSE('',#9734,0.0216399563664949,0.02) ;
#169 = ELLIPSE('',#9736,0.021639956366495,0.02) ;
#170 = ELLIPSE('',#9737,0.021639956366495,0.02) ;
#171 = ELLIPSE('',#9739,0.0216399563664949,0.02) ;
#172 = ELLIPSE('',#9740,0.0216399563664949,0.02) ;
#173 = ELLIPSE('',#9741,0.0216399563664949,0.02) ;
#174 = ELLIPSE('',#9743,0.0216399563664949,0.02) ;
#175 = ELLIPSE('',#9744,0.0216399563664949,0.02) ;
#176 = ELLIPSE('',#9746,0.0216399563664949,0.02) ;
#177 = ELLIPSE('',#9747,0.0216399563664949,0.02) ;
#178 = ELLIPSE('',#9748,0.0216399563664949,0.02) ;
#179 = ELLIPSE('',#9750,0.021639956366495,0.02) ;
#180 = ELLIPSE('',#9751,0.021639956366495,0.02) ;
#181 = ELLIPSE('',#9753,0.0216399563664949,0.02) ;
#182 = ELLIPSE('',#9755,0.0216399563664949,0.02) ;
#183 = ELLIPSE('',#9757,0.0216399563664948,0.02) ;
#184 = ELLIPSE('',#9759,0.021639956366495,0.02) ;
#185 = ELLIPSE('',#9760,0.021639956366495,0.02) ;
#186 = ELLIPSE('',#9762,0.0216399563664949,0.02) ;
#187 = ELLIPSE('',#9763,0.0216399563664949,0.02) ;
#188 = ELLIPSE('',#9764,0.0216399563664949,0.02) ;
#189 = ORIENTED_CLOSED_SHELL('',*,#8262,.F.) ;
#190 = ORIENTED_CLOSED_SHELL('',*,#8263,.F.) ;
#191 = BREP_WITH_VOIDS('INTERNAL_STEAM_TUBE_CONDUIT',#8264,(#189,#190)) ;
#192 = SPHERICAL_SURFACE('',#8859,0.25) ;
#193 = SPHERICAL_SURFACE('',#8933,0.3) ;
#194 = SPHERICAL_SURFACE('',#8935,0.4) ;
#195 = SPHERICAL_SURFACE('',#8964,0.4) ;
#196 = SPHERICAL_SURFACE('',#8965,0.4) ;
#197 = SPHERICAL_SURFACE('',#8966,0.4) ;
#198 = SPHERICAL_SURFACE('',#9045,0.025) ;
#199 = SPHERICAL_SURFACE('',#9048,0.025) ;
#200 = SPHERICAL_SURFACE('',#9052,0.025) ;
#201 = SPHERICAL_SURFACE('',#9057,0.025) ;
#202 = SPHERICAL_SURFACE('',#9062,0.025) ;
#203 = SPHERICAL_SURFACE('',#9067,0.025) ;
#204 = SPHERICAL_SURFACE('',#9071,0.025) ;
#205 = SPHERICAL_SURFACE('',#9074,0.025) ;
#206 = SPHERICAL_SURFACE('',#9077,0.025) ;
#207 = SPHERICAL_SURFACE('',#9080,0.025) ;
#208 = SPHERICAL_SURFACE('',#9084,0.025) ;
#209 = SPHERICAL_SURFACE('',#9089,0.025) ;
#210 = SPHERICAL_SURFACE('',#9094,0.025) ;
#211 = SPHERICAL_SURFACE('',#9099,0.025) ;
#212 = SPHERICAL_SURFACE('',#9103,0.025) ;
#213 = SPHERICAL_SURFACE('',#9106,0.025) ;
#214 = SPHERICAL_SURFACE('',#9109,0.025) ;
#215 = SPHERICAL_SURFACE('',#9112,0.025) ;
#216 = SPHERICAL_SURFACE('',#9116,0.025) ;
#217 = SPHERICAL_SURFACE('',#9121,0.025) ;
#218 = SPHERICAL_SURFACE('',#9126,0.025) ;
#219 = SPHERICAL_SURFACE('',#9131,0.025) ;
#220 = SPHERICAL_SURFACE('',#9135,0.025) ;
#221 = SPHERICAL_SURFACE('',#9138,0.025) ;
#222 = SPHERICAL_SURFACE('',#9141,0.025) ;
#223 = SPHERICAL_SURFACE('',#9144,0.025) ;
#224 = SPHERICAL_SURFACE('',#9148,0.025) ;
#225 = SPHERICAL_SURFACE('',#9153,0.025) ;
#226 = SPHERICAL_SURFACE('',#9158,0.025) ;
#227 = SPHERICAL_SURFACE('',#9163,0.025) ;
#228 = SPHERICAL_SURFACE('',#9167,0.025) ;
#229 = SPHERICAL_SURFACE('',#9170,0.025) ;
#230 = SPHERICAL_SURFACE('',#9173,0.025) ;
#231 = SPHERICAL_SURFACE('',#9176,0.025) ;
#232 = SPHERICAL_SURFACE('',#9180,0.025) ;
#233 = SPHERICAL_SURFACE('',#9185,0.025) ;
#234 = SPHERICAL_SURFACE('',#9190,0.025) ;
#235 = SPHERICAL_SURFACE('',#9195,0.025) ;
#236 = SPHERICAL_SURFACE('',#9199,0.025) ;
#237 = SPHERICAL_SURFACE('',#9350,0.025) ;
#238 = SPHERICAL_SURFACE('',#9353,0.025) ;
#239 = SPHERICAL_SURFACE('',#9357,0.025) ;
#240 = SPHERICAL_SURFACE('',#9362,0.025) ;
#241 = SPHERICAL_SURFACE('',#9367,0.025) ;
#242 = SPHERICAL_SURFACE('',#9372,0.025) ;
#243 = SPHERICAL_SURFACE('',#9376,0.025) ;
#244 = SPHERICAL_SURFACE('',#9379,0.025) ;
#245 = SPHERICAL_SURFACE('',#9382,0.025) ;
#246 = SPHERICAL_SURFACE('',#9385,0.025) ;
#247 = SPHERICAL_SURFACE('',#9389,0.025) ;
#248 = SPHERICAL_SURFACE('',#9394,0.025) ;
#249 = SPHERICAL_SURFACE('',#9399,0.025) ;
#250 = SPHERICAL_SURFACE('',#9404,0.025) ;
#251 = SPHERICAL_SURFACE('',#9408,0.025) ;
#252 = SPHERICAL_SURFACE('',#9411,0.025) ;
#253 = SPHERICAL_SURFACE('',#9414,0.025) ;
#254 = SPHERICAL_SURFACE('',#9417,0.025) ;
#255 = SPHERICAL_SURFACE('',#9421,0.025) ;
#256 = SPHERICAL_SURFACE('',#9426,0.025) ;
#257 = SPHERICAL_SURFACE('',#9431,0.025) ;
#258 = SPHERICAL_SURFACE('',#9436,0.025) ;
#259 = SPHERICAL_SURFACE('',#9440,0.025) ;
#260 = SPHERICAL_SURFACE('',#9549,0.02) ;
#261 = SPHERICAL_SURFACE('',#9552,0.02) ;
#262 = SPHERICAL_SURFACE('',#9556,0.02) ;
#263 = SPHERICAL_SURFACE('',#9561,0.02) ;
#264 = SPHERICAL_SURFACE('',#9566,0.02) ;
#265 = SPHERICAL_SURFACE('',#9571,0.02) ;
#266 = SPHERICAL_SURFACE('',#9575,0.02) ;
#267 = SPHERICAL_SURFACE('',#9578,0.02) ;
#268 = SPHERICAL_SURFACE('',#9581,0.02) ;
#269 = SPHERICAL_SURFACE('',#9584,0.02) ;
#270 = SPHERICAL_SURFACE('',#9588,0.02) ;
#271 = SPHERICAL_SURFACE('',#9593,0.02) ;
#272 = SPHERICAL_SURFACE('',#9598,0.02) ;
#273 = SPHERICAL_SURFACE('',#9603,0.02) ;
#274 = SPHERICAL_SURFACE('',#9607,0.02) ;
#275 = SPHERICAL_SURFACE('',#9610,0.02) ;
#276 = SPHERICAL_SURFACE('',#9613,0.02) ;
#277 = SPHERICAL_SURFACE('',#9616,0.02) ;
#278 = SPHERICAL_SURFACE('',#9620,0.02) ;
#279 = SPHERICAL_SURFACE('',#9625,0.02) ;
#280 = SPHERICAL_SURFACE('',#9630,0.02) ;
#281 = SPHERICAL_SURFACE('',#9635,0.02) ;
#282 = SPHERICAL_SURFACE('',#9639,0.02) ;
#283 = SPHERICAL_SURFACE('',#9642,0.02) ;
#284 = SPHERICAL_SURFACE('',#9645,0.02) ;
#285 = SPHERICAL_SURFACE('',#9648,0.02) ;
#286 = SPHERICAL_SURFACE('',#9652,0.02) ;
#287 = SPHERICAL_SURFACE('',#9657,0.02) ;
#288 = SPHERICAL_SURFACE('',#9662,0.02) ;
#289 = SPHERICAL_SURFACE('',#9667,0.02) ;
#290 = SPHERICAL_SURFACE('',#9671,0.02) ;
#291 = SPHERICAL_SURFACE('',#9810,0.15) ;
#292 = SPHERICAL_SURFACE('',#9813,0.15) ;
#293 = ITEM_DEFINED_TRANSFORMATION($,$,#8684,#8796) ;
#294 = ITEM_DEFINED_TRANSFORMATION($,$,#8764,#8797) ;
#295 = ITEM_DEFINED_TRANSFORMATION($,$,#8799,#8865) ;
#296 = ITEM_DEFINED_TRANSFORMATION($,$,#8840,#8866) ;
#297 = ITEM_DEFINED_TRANSFORMATION($,$,#8849,#8867) ;
#298 = ITEM_DEFINED_TRANSFORMATION($,$,#8858,#8868) ;
#299 = ITEM_DEFINED_TRANSFORMATION($,$,#8870,#9001) ;
#300 = ITEM_DEFINED_TRANSFORMATION($,$,#8883,#9002) ;
#301 = ITEM_DEFINED_TRANSFORMATION($,$,#8893,#9003) ;
#302 = ITEM_DEFINED_TRANSFORMATION($,$,#8899,#9004) ;
#303 = ITEM_DEFINED_TRANSFORMATION($,$,#8932,#9005) ;
#304 = ITEM_DEFINED_TRANSFORMATION($,$,#8967,#9006) ;
#305 = ITEM_DEFINED_TRANSFORMATION($,$,#8976,#9007) ;
#306 = ITEM_DEFINED_TRANSFORMATION($,$,#8989,#9008) ;
#307 = ITEM_DEFINED_TRANSFORMATION($,$,#8995,#9009) ;
#308 = ITEM_DEFINED_TRANSFORMATION($,$,#9011,#9768) ;
#309 = ITEM_DEFINED_TRANSFORMATION($,$,#9034,#9769) ;
#310 = ITEM_DEFINED_TRANSFORMATION($,$,#9044,#9770) ;
#311 = ITEM_DEFINED_TRANSFORMATION($,$,#9319,#9771) ;
#312 = ITEM_DEFINED_TRANSFORMATION($,$,#9333,#9772) ;
#313 = ITEM_DEFINED_TRANSFORMATION($,$,#9349,#9773) ;
#314 = ITEM_DEFINED_TRANSFORMATION($,$,#9514,#9774) ;
#315 = ITEM_DEFINED_TRANSFORMATION($,$,#9525,#9775) ;
#316 = ITEM_DEFINED_TRANSFORMATION($,$,#9536,#9776) ;
#317 = ITEM_DEFINED_TRANSFORMATION($,$,#9542,#9777) ;
#318 = ITEM_DEFINED_TRANSFORMATION($,$,#9548,#9778) ;
#319 = ITEM_DEFINED_TRANSFORMATION($,$,#9780,#9885) ;
#320 = ITEM_DEFINED_TRANSFORMATION($,$,#9780,#9886) ;
#321 = ITEM_DEFINED_TRANSFORMATION($,$,#9780,#9887) ;
#322 = ITEM_DEFINED_TRANSFORMATION($,$,#9794,#9888) ;
#323 = ITEM_DEFINED_TRANSFORMATION($,$,#9809,#9889) ;
#324 = ITEM_DEFINED_TRANSFORMATION($,$,#9828,#9890) ;
#325 = ITEM_DEFINED_TRANSFORMATION($,$,#9844,#9891) ;
#326 = ITEM_DEFINED_TRANSFORMATION($,$,#9863,#9892) ;
#327 = ITEM_DEFINED_TRANSFORMATION($,$,#9879,#9893) ;
#328 = ITEM_DEFINED_TRANSFORMATION($,$,#9895,#9915) ;
#329 = ITEM_DEFINED_TRANSFORMATION($,$,#9895,#9916) ;
#330 = ITEM_DEFINED_TRANSFORMATION($,$,#9905,#9917) ;
#331 = ITEM_DEFINED_TRANSFORMATION($,$,#9905,#9918) ;
#332 = ITEM_DEFINED_TRANSFORMATION($,$,#8683,#9919) ;
#333 = ITEM_DEFINED_TRANSFORMATION($,$,#8798,#9920) ;
#334 = ITEM_DEFINED_TRANSFORMATION($,$,#8869,#9921) ;
#335 = ITEM_DEFINED_TRANSFORMATION($,$,#9010,#9922) ;
#336 = ITEM_DEFINED_TRANSFORMATION($,$,#9779,#9923) ;
#337 = ITEM_DEFINED_TRANSFORMATION($,$,#9894,#9924) ;
#338 = (
REPRESENTATION_RELATIONSHIP($,$,#15620,#15619)
REPRESENTATION_RELATIONSHIP_WITH_TRANSFORMATION(#293)
SHAPE_REPRESENTATION_RELATIONSHIP()
) ;
#339 = (
REPRESENTATION_RELATIONSHIP($,$,#15621,#15619)
REPRESENTATION_RELATIONSHIP_WITH_TRANSFORMATION(#294)
SHAPE_REPRESENTATION_RELATIONSHIP()
) ;
#340 = (
REPRESENTATION_RELATIONSHIP($,$,#15623,#15622)
REPRESENTATION_RELATIONSHIP_WITH_TRANSFORMATION(#295)
SHAPE_REPRESENTATION_RELATIONSHIP()
) ;
#341 = (
REPRESENTATION_RELATIONSHIP($,$,#15624,#15622)
REPRESENTATION_RELATIONSHIP_WITH_TRANSFORMATION(#296)
SHAPE_REPRESENTATION_RELATIONSHIP()
) ;
#342 = (
REPRESENTATION_RELATIONSHIP($,$,#15625,#15622)
REPRESENTATION_RELATIONSHIP_WITH_TRANSFORMATION(#297)
SHAPE_REPRESENTATION_RELATIONSHIP()
) ;
#343 = (
REPRESENTATION_RELATIONSHIP($,$,#15626,#15622)
REPRESENTATION_RELATIONSHIP_WITH_TRANSFORMATION(#298)
SHAPE_REPRESENTATION_RELATIONSHIP()
) ;
#344 = (
REPRESENTATION_RELATIONSHIP($,$,#15628,#15627)
REPRESENTATION_RELATIONSHIP_WITH_TRANSFORMATION(#299)
SHAPE_REPRESENTATION_RELATIONSHIP()
) ;
#345 = (
REPRESENTATION_RELATIONSHIP($,$,#15629,#15627)
REPRESENTATION_RELATIONSHIP_WITH_TRANSFORMATION(#300)
SHAPE_REPRESENTATION_RELATIONSHIP()
) ;
#346 = (
REPRESENTATION_RELATIONSHIP($,$,#15630,#15627)
REPRESENTATION_RELATIONSHIP_WITH_TRANSFORMATION(#301)
SHAPE_REPRESENTATION_RELATIONSHIP()
) ;
#347 = (
REPRESENTATION_RELATIONSHIP($,$,#15631,#15627)
REPRESENTATION_RELATIONSHIP_WITH_TRANSFORMATION(#302)
SHAPE_REPRESENTATION_RELATIONSHIP()
) ;
#348 = (
REPRESENTATION_RELATIONSHIP($,$,#15632,#15627)
REPRESENTATION_RELATIONSHIP_WITH_TRANSFORMATION(#303)
SHAPE_REPRESENTATION_RELATIONSHIP()
) ;
#349 = (
REPRESENTATION_RELATIONSHIP($,$,#15633,#15627)
REPRESENTATION_RELATIONSHIP_WITH_TRANSFORMATION(#304)
SHAPE_REPRESENTATION_RELATIONSHIP()
) ;
#350 = (
REPRESENTATION_RELATIONSHIP($,$,#15634,#15627)
REPRESENTATION_RELATIONSHIP_WITH_TRANSFORMATION(#305)
SHAPE_REPRESENTATION_RELATIONSHIP()
) ;
#351 = (
REPRESENTATION_RELATIONSHIP($,$,#15635,#15627)
REPRESENTATION_RELATIONSHIP_WITH_TRANSFORMATION(#306)
SHAPE_REPRESENTATION_RELATIONSHIP()
) ;
#352 = (
REPRESENTATION_RELATIONSHIP($,$,#15636,#15627)
REPRESENTATION_RELATIONSHIP_WITH_TRANSFORMATION(#307)
SHAPE_REPRESENTATION_RELATIONSHIP()
) ;
#353 = (
REPRESENTATION_RELATIONSHIP($,$,#15638,#15637)
REPRESENTATION_RELATIONSHIP_WITH_TRANSFORMATION(#308)
SHAPE_REPRESENTATION_RELATIONSHIP()
) ;
#354 = (
REPRESENTATION_RELATIONSHIP($,$,#15639,#15637)
REPRESENTATION_RELATIONSHIP_WITH_TRANSFORMATION(#309)
SHAPE_REPRESENTATION_RELATIONSHIP()
) ;
#355 = (
REPRESENTATION_RELATIONSHIP($,$,#15640,#15637)
REPRESENTATION_RELATIONSHIP_WITH_TRANSFORMATION(#310)
SHAPE_REPRESENTATION_RELATIONSHIP()
) ;
#356 = (
REPRESENTATION_RELATIONSHIP($,$,#15641,#15637)
REPRESENTATION_RELATIONSHIP_WITH_TRANSFORMATION(#311)
SHAPE_REPRESENTATION_RELATIONSHIP()
) ;
#357 = (
REPRESENTATION_RELATIONSHIP($,$,#15642,#15637)
REPRESENTATION_RELATIONSHIP_WITH_TRANSFORMATION(#312)
SHAPE_REPRESENTATION_RELATIONSHIP()
) ;
#358 = (
REPRESENTATION_RELATIONSHIP($,$,#15643,#15637)
REPRESENTATION_RELATIONSHIP_WITH_TRANSFORMATION(#313)
SHAPE_REPRESENTATION_RELATIONSHIP()
) ;
#359 = (
REPRESENTATION_RELATIONSHIP($,$,#15644,#15637)
REPRESENTATION_RELATIONSHIP_WITH_TRANSFORMATION(#314)
SHAPE_REPRESENTATION_RELATIONSHIP()
) ;
#360 = (
REPRESENTATION_RELATIONSHIP($,$,#15645,#15637)
REPRESENTATION_RELATIONSHIP_WITH_TRANSFORMATION(#315)
SHAPE_REPRESENTATION_RELATIONSHIP()
) ;
#361 = (
REPRESENTATION_RELATIONSHIP($,$,#15646,#15637)
REPRESENTATION_RELATIONSHIP_WITH_TRANSFORMATION(#316)
SHAPE_REPRESENTATION_RELATIONSHIP()
) ;
#362 = (
REPRESENTATION_RELATIONSHIP($,$,#15647,#15637)
REPRESENTATION_RELATIONSHIP_WITH_TRANSFORMATION(#317)
SHAPE_REPRESENTATION_RELATIONSHIP()
) ;
#363 = (
REPRESENTATION_RELATIONSHIP($,$,#15648,#15637)
REPRESENTATION_RELATIONSHIP_WITH_TRANSFORMATION(#318)
SHAPE_REPRESENTATION_RELATIONSHIP()
) ;
#364 = (
REPRESENTATION_RELATIONSHIP($,$,#15650,#15649)
REPRESENTATION_RELATIONSHIP_WITH_TRANSFORMATION(#319)
SHAPE_REPRESENTATION_RELATIONSHIP()
) ;
#365 = (
REPRESENTATION_RELATIONSHIP($,$,#15650,#15649)
REPRESENTATION_RELATIONSHIP_WITH_TRANSFORMATION(#320)
SHAPE_REPRESENTATION_RELATIONSHIP()
) ;
#366 = (
REPRESENTATION_RELATIONSHIP($,$,#15650,#15649)
REPRESENTATION_RELATIONSHIP_WITH_TRANSFORMATION(#321)
SHAPE_REPRESENTATION_RELATIONSHIP()
) ;
#367 = (
REPRESENTATION_RELATIONSHIP($,$,#15651,#15649)
REPRESENTATION_RELATIONSHIP_WITH_TRANSFORMATION(#322)
SHAPE_REPRESENTATION_RELATIONSHIP()
) ;
#368 = (
REPRESENTATION_RELATIONSHIP($,$,#15652,#15649)
REPRESENTATION_RELATIONSHIP_WITH_TRANSFORMATION(#323)
SHAPE_REPRESENTATION_RELATIONSHIP()
) ;
#369 = (
REPRESENTATION_RELATIONSHIP($,$,#15653,#15649)
REPRESENTATION_RELATIONSHIP_WITH_TRANSFORMATION(#324)
SHAPE_REPRESENTATION_RELATIONSHIP()
) ;
#370 = (
REPRESENTATION_RELATIONSHIP($,$,#15654,#15649)
REPRESENTATION_RELATIONSHIP_WITH_TRANSFORMATION(#325)
SHAPE_REPRESENTATION_RELATIONSHIP()
) ;
#371 = (
REPRESENTATION_RELATIONSHIP($,$,#15655,#15649)
REPRESENTATION_RELATIONSHIP_WITH_TRANSFORMATION(#326)
SHAPE_REPRESENTATION_RELATIONSHIP()
) ;
#372 = (
REPRESENTATION_RELATIONSHIP($,$,#15656,#15649)
REPRESENTATION_RELATIONSHIP_WITH_TRANSFORMATION(#327)
SHAPE_REPRESENTATION_RELATIONSHIP()
) ;
#373 = (
REPRESENTATION_RELATIONSHIP($,$,#15658,#15657)
REPRESENTATION_RELATIONSHIP_WITH_TRANSFORMATION(#328)
SHAPE_REPRESENTATION_RELATIONSHIP()
) ;
#374 = (
REPRESENTATION_RELATIONSHIP($,$,#15658,#15657)
REPRESENTATION_RELATIONSHIP_WITH_TRANSFORMATION(#329)
SHAPE_REPRESENTATION_RELATIONSHIP()
) ;
#375 = (
REPRESENTATION_RELATIONSHIP($,$,#15659,#15657)
REPRESENTATION_RELATIONSHIP_WITH_TRANSFORMATION(#330)
SHAPE_REPRESENTATION_RELATIONSHIP()
) ;
#376 = (
REPRESENTATION_RELATIONSHIP($,$,#15659,#15657)
REPRESENTATION_RELATIONSHIP_WITH_TRANSFORMATION(#331)
SHAPE_REPRESENTATION_RELATIONSHIP()
) ;
#377 = (
REPRESENTATION_RELATIONSHIP($,$,#15619,#15618)
REPRESENTATION_RELATIONSHIP_WITH_TRANSFORMATION(#332)
SHAPE_REPRESENTATION_RELATIONSHIP()
) ;
#378 = (
REPRESENTATION_RELATIONSHIP($,$,#15622,#15618)
REPRESENTATION_RELATIONSHIP_WITH_TRANSFORMATION(#333)
SHAPE_REPRESENTATION_RELATIONSHIP()
) ;
#379 = (
REPRESENTATION_RELATIONSHIP($,$,#15627,#15618)
REPRESENTATION_RELATIONSHIP_WITH_TRANSFORMATION(#334)
SHAPE_REPRESENTATION_RELATIONSHIP()
) ;
#380 = (
REPRESENTATION_RELATIONSHIP($,$,#15637,#15618)
REPRESENTATION_RELATIONSHIP_WITH_TRANSFORMATION(#335)
SHAPE_REPRESENTATION_RELATIONSHIP()
) ;
#381 = (
REPRESENTATION_RELATIONSHIP($,$,#15649,#15618)
REPRESENTATION_RELATIONSHIP_WITH_TRANSFORMATION(#336)
SHAPE_REPRESENTATION_RELATIONSHIP()
) ;
#382 = (
REPRESENTATION_RELATIONSHIP($,$,#15657,#15618)
REPRESENTATION_RELATIONSHIP_WITH_TRANSFORMATION(#337)
SHAPE_REPRESENTATION_RELATIONSHIP()
) ;
#383 = CONTEXT_DEPENDENT_SHAPE_REPRESENTATION(#338,#15535) ;
#384 = CONTEXT_DEPENDENT_SHAPE_REPRESENTATION(#339,#15536) ;
#385 = CONTEXT_DEPENDENT_SHAPE_REPRESENTATION(#340,#15542) ;
#386 = CONTEXT_DEPENDENT_SHAPE_REPRESENTATION(#341,#15543) ;
#387 = CONTEXT_DEPENDENT_SHAPE_REPRESENTATION(#342,#15544) ;
#388 = CONTEXT_DEPENDENT_SHAPE_REPRESENTATION(#343,#15545) ;
#389 = CONTEXT_DEPENDENT_SHAPE_REPRESENTATION(#344,#15556) ;
#390 = CONTEXT_DEPENDENT_SHAPE_REPRESENTATION(#345,#15557) ;
#391 = CONTEXT_DEPENDENT_SHAPE_REPRESENTATION(#346,#15558) ;
#392 = CONTEXT_DEPENDENT_SHAPE_REPRESENTATION(#347,#15559) ;
#393 = CONTEXT_DEPENDENT_SHAPE_REPRESENTATION(#348,#15560) ;
#394 = CONTEXT_DEPENDENT_SHAPE_REPRESENTATION(#349,#15561) ;
#395 = CONTEXT_DEPENDENT_SHAPE_REPRESENTATION(#350,#15562) ;
#396 = CONTEXT_DEPENDENT_SHAPE_REPRESENTATION(#351,#15563) ;
#397 = CONTEXT_DEPENDENT_SHAPE_REPRESENTATION(#352,#15564) ;
#398 = CONTEXT_DEPENDENT_SHAPE_REPRESENTATION(#353,#15577) ;
#399 = CONTEXT_DEPENDENT_SHAPE_REPRESENTATION(#354,#15578) ;
#400 = CONTEXT_DEPENDENT_SHAPE_REPRESENTATION(#355,#15579) ;
#401 = CONTEXT_DEPENDENT_SHAPE_REPRESENTATION(#356,#15580) ;
#402 = CONTEXT_DEPENDENT_SHAPE_REPRESENTATION(#357,#15581) ;
#403 = CONTEXT_DEPENDENT_SHAPE_REPRESENTATION(#358,#15582) ;
#404 = CONTEXT_DEPENDENT_SHAPE_REPRESENTATION(#359,#15583) ;
#405 = CONTEXT_DEPENDENT_SHAPE_REPRESENTATION(#360,#15584) ;
#406 = CONTEXT_DEPENDENT_SHAPE_REPRESENTATION(#361,#15585) ;
#407 = CONTEXT_DEPENDENT_SHAPE_REPRESENTATION(#362,#15586) ;
#408 = CONTEXT_DEPENDENT_SHAPE_REPRESENTATION(#363,#15587) ;
#409 = CONTEXT_DEPENDENT_SHAPE_REPRESENTATION(#364,#15596) ;
#410 = CONTEXT_DEPENDENT_SHAPE_REPRESENTATION(#365,#15597) ;
#411 = CONTEXT_DEPENDENT_SHAPE_REPRESENTATION(#366,#15598) ;
#412 = CONTEXT_DEPENDENT_SHAPE_REPRESENTATION(#367,#15599) ;
#413 = CONTEXT_DEPENDENT_SHAPE_REPRESENTATION(#368,#15600) ;
#414 = CONTEXT_DEPENDENT_SHAPE_REPRESENTATION(#369,#15601) ;
#415 = CONTEXT_DEPENDENT_SHAPE_REPRESENTATION(#370,#15602) ;
#416 = CONTEXT_DEPENDENT_SHAPE_REPRESENTATION(#371,#15603) ;
#417 = CONTEXT_DEPENDENT_SHAPE_REPRESENTATION(#372,#15604) ;
#418 = CONTEXT_DEPENDENT_SHAPE_REPRESENTATION(#373,#15608) ;
#419 = CONTEXT_DEPENDENT_SHAPE_REPRESENTATION(#374,#15609) ;
#420 = CONTEXT_DEPENDENT_SHAPE_REPRESENTATION(#375,#15610) ;
#421 = CONTEXT_DEPENDENT_SHAPE_REPRESENTATION(#376,#15611) ;
#422 = CONTEXT_DEPENDENT_SHAPE_REPRESENTATION(#377,#15612) ;
#423 = CONTEXT_DEPENDENT_SHAPE_REPRESENTATION(#378,#15613) ;
#424 = CONTEXT_DEPENDENT_SHAPE_REPRESENTATION(#379,#15614) ;
#425 = CONTEXT_DEPENDENT_SHAPE_REPRESENTATION(#380,#15615) ;
#426 = CONTEXT_DEPENDENT_SHAPE_REPRESENTATION(#381,#15616) ;
#427 = CONTEXT_DEPENDENT_SHAPE_REPRESENTATION(#382,#15617) ;
#428 = NEXT_ASSEMBLY_USAGE_OCCURRENCE('CONTROL_HOUSING_BODY:1',
'CONTROL_HOUSING_BODY:1','CONTROL_HOUSING_BODY:1',#15662,#15663,
'CONTROL_HOUSING_BODY:1') ;
#429 = NEXT_ASSEMBLY_USAGE_OCCURRENCE('BASE_STATION_CORD_RETAINER:1',
'BASE_STATION_CORD_RETAINER:1','BASE_STATION_CORD_RETAINER:1',#15662,#15664,
'BASE_STATION_CORD_RETAINER:1') ;
#430 = NEXT_ASSEMBLY_USAGE_OCCURRENCE(
'STANDARD_3PIN_STRIX_CONNECTOR_BASE:1',
'STANDARD_3PIN_STRIX_CONNECTOR_BASE:1',
'STANDARD_3PIN_STRIX_CONNECTOR_BASE:1',#15665,#15666,
'STANDARD_3PIN_STRIX_CONNECTOR_BASE:1') ;
#431 = NEXT_ASSEMBLY_USAGE_OCCURRENCE('EARTH_CONTACT_RING:1',
'EARTH_CONTACT_RING:1','EARTH_CONTACT_RING:1',#15665,#15667,
'EARTH_CONTACT_RING:1') ;
#432 = NEXT_ASSEMBLY_USAGE_OCCURRENCE('LIVE_CONTACT_RING:1',
'LIVE_CONTACT_RING:1','LIVE_CONTACT_RING:1',#15665,#15668,
'LIVE_CONTACT_RING:1') ;
#433 = NEXT_ASSEMBLY_USAGE_OCCURRENCE('NEUTRAL_CENTRE_PIN:1',
'NEUTRAL_CENTRE_PIN:1','NEUTRAL_CENTRE_PIN:1',#15665,#15669,
'NEUTRAL_CENTRE_PIN:1') ;
#434 = NEXT_ASSEMBLY_USAGE_OCCURRENCE('STEAM_DISC_HOLDER_CUP:1',
'STEAM_DISC_HOLDER_CUP:1','STEAM_DISC_HOLDER_CUP:1',#15670,#15671,
'STEAM_DISC_HOLDER_CUP:1') ;
#435 = NEXT_ASSEMBLY_USAGE_OCCURRENCE(
'BIMETALLIC_THERMOSTATIC_DISC_UNIT:1',
'BIMETALLIC_THERMOSTATIC_DISC_UNIT:1',
'BIMETALLIC_THERMOSTATIC_DISC_UNIT:1',#15670,#15672,
'BIMETALLIC_THERMOSTATIC_DISC_UNIT:1') ;
#436 = NEXT_ASSEMBLY_USAGE_OCCURRENCE('STEAM_DISC_PUSH_ROD:1',
'STEAM_DISC_PUSH_ROD:1','STEAM_DISC_PUSH_ROD:1',#15670,#15673,
'STEAM_DISC_PUSH_ROD:1') ;
#437 = NEXT_ASSEMBLY_USAGE_OCCURRENCE('STEAM_PORT_DEFLECTOR_CAP:1',
'STEAM_PORT_DEFLECTOR_CAP:1','STEAM_PORT_DEFLECTOR_CAP:1',#15670,#15674,
'STEAM_PORT_DEFLECTOR_CAP:1') ;
#438 = NEXT_ASSEMBLY_USAGE_OCCURRENCE('INTERNAL_STEAM_TUBE_CONDUIT:1',
'INTERNAL_STEAM_TUBE_CONDUIT:1','INTERNAL_STEAM_TUBE_CONDUIT:1',#15670,
#15675,'INTERNAL_STEAM_TUBE_CONDUIT:1') ;
#439 = NEXT_ASSEMBLY_USAGE_OCCURRENCE('STEAM_SEAL_GROMMET:1',
'STEAM_SEAL_GROMMET:1','STEAM_SEAL_GROMMET:1',#15670,#15676,
'STEAM_SEAL_GROMMET:1') ;
#440 = NEXT_ASSEMBLY_USAGE_OCCURRENCE('DRY_BOIL_DISC_HOLDER:1',
'DRY_BOIL_DISC_HOLDER:1','DRY_BOIL_DISC_HOLDER:1',#15670,#15677,
'DRY_BOIL_DISC_HOLDER:1') ;
#441 = NEXT_ASSEMBLY_USAGE_OCCURRENCE('DRY_BOIL_BIMETAL_DISC:1',
'DRY_BOIL_BIMETAL_DISC:1','DRY_BOIL_BIMETAL_DISC:1',#15670,#15678,
'DRY_BOIL_BIMETAL_DISC:1') ;
#442 = NEXT_ASSEMBLY_USAGE_OCCURRENCE('DRY_BOIL_PUSH_ROD:1',
'DRY_BOIL_PUSH_ROD:1','DRY_BOIL_PUSH_ROD:1',#15670,#15679,
'DRY_BOIL_PUSH_ROD:1') ;
#443 = NEXT_ASSEMBLY_USAGE_OCCURRENCE('AUTO_OFF_LATCH_TRIP_LEVER:1',
'AUTO_OFF_LATCH_TRIP_LEVER:1','AUTO_OFF_LATCH_TRIP_LEVER:1',#15680,#15681,
'AUTO_OFF_LATCH_TRIP_LEVER:1') ;
#444 = NEXT_ASSEMBLY_USAGE_OCCURRENCE('TRIP_LEVER_PIVOT_PIN:1',
'TRIP_LEVER_PIVOT_PIN:1','TRIP_LEVER_PIVOT_PIN:1',#15680,#15682,
'TRIP_LEVER_PIVOT_PIN:1') ;
#445 = NEXT_ASSEMBLY_USAGE_OCCURRENCE('TRIP_LEVER_RETURN_SPRING:1',
'TRIP_LEVER_RETURN_SPRING:1','TRIP_LEVER_RETURN_SPRING:1',#15680,#15683,
'TRIP_LEVER_RETURN_SPRING:1') ;
#446 = NEXT_ASSEMBLY_USAGE_OCCURRENCE('PUSH_BUTTON_STEM:1',
'PUSH_BUTTON_STEM:1','PUSH_BUTTON_STEM:1',#15680,#15684,
'PUSH_BUTTON_STEM:1') ;
#447 = NEXT_ASSEMBLY_USAGE_OCCURRENCE('PUSH_BUTTON_CAP:1',
'PUSH_BUTTON_CAP:1','PUSH_BUTTON_CAP:1',#15680,#15685,
'PUSH_BUTTON_CAP:1') ;
#448 = NEXT_ASSEMBLY_USAGE_OCCURRENCE('BUTTON_RETURN_SPRING:1',
'BUTTON_RETURN_SPRING:1','BUTTON_RETURN_SPRING:1',#15680,#15686,
'BUTTON_RETURN_SPRING:1') ;
#449 = NEXT_ASSEMBLY_USAGE_OCCURRENCE('MOVING_CONTACT_ARM:1',
'MOVING_CONTACT_ARM:1','MOVING_CONTACT_ARM:1',#15680,#15687,
'MOVING_CONTACT_ARM:1') ;
#450 = NEXT_ASSEMBLY_USAGE_OCCURRENCE('CONTACT_ANCHOR_POST:1',
'CONTACT_ANCHOR_POST:1','CONTACT_ANCHOR_POST:1',#15680,#15688,
'CONTACT_ANCHOR_POST:1') ;
#451 = NEXT_ASSEMBLY_USAGE_OCCURRENCE('FIXED_CONTACT_POST:1',
'FIXED_CONTACT_POST:1','FIXED_CONTACT_POST:1',#15680,#15689,
'FIXED_CONTACT_POST:1') ;
#452 = NEXT_ASSEMBLY_USAGE_OCCURRENCE('CONTACT_RIVET_SILVER:1',
'CONTACT_RIVET_SILVER:1','CONTACT_RIVET_SILVER:1',#15680,#15690,
'CONTACT_RIVET_SILVER:1') ;
#453 = NEXT_ASSEMBLY_USAGE_OCCURRENCE('CONTACT_PRESSURE_SPRING:1',
'CONTACT_PRESSURE_SPRING:1','CONTACT_PRESSURE_SPRING:1',#15680,#15691,
'CONTACT_PRESSURE_SPRING:1') ;
#454 = NEXT_ASSEMBLY_USAGE_OCCURRENCE('ELECTRICAL_TERMINAL_CONTACT_PIN:1',
'ELECTRICAL_TERMINAL_CONTACT_PIN:1','ELECTRICAL_TERMINAL_CONTACT_PIN:1',
#15692,#15693,'ELECTRICAL_TERMINAL_CONTACT_PIN:1') ;
#455 = NEXT_ASSEMBLY_USAGE_OCCURRENCE('ELECTRICAL_TERMINAL_CONTACT_PIN:2',
'ELECTRICAL_TERMINAL_CONTACT_PIN:2','ELECTRICAL_TERMINAL_CONTACT_PIN:2',
#15692,#15693,'ELECTRICAL_TERMINAL_CONTACT_PIN:2') ;
#456 = NEXT_ASSEMBLY_USAGE_OCCURRENCE('ELECTRICAL_TERMINAL_CONTACT_PIN:3',
'ELECTRICAL_TERMINAL_CONTACT_PIN:3','ELECTRICAL_TERMINAL_CONTACT_PIN:3',
#15692,#15693,'ELECTRICAL_TERMINAL_CONTACT_PIN:3') ;
#457 = NEXT_ASSEMBLY_USAGE_OCCURRENCE('INDICATOR_LED_LIGHT_HOUSING:1',
'INDICATOR_LED_LIGHT_HOUSING:1','INDICATOR_LED_LIGHT_HOUSING:1',#15692,
#15694,'INDICATOR_LED_LIGHT_HOUSING:1') ;
#458 = NEXT_ASSEMBLY_USAGE_OCCURRENCE('LED_LAMP:1','LED_LAMP:1',
'LED_LAMP:1',#15692,#15695,'LED_LAMP:1') ;
#459 = NEXT_ASSEMBLY_USAGE_OCCURRENCE('LED_SERIES_RESISTOR:1',
'LED_SERIES_RESISTOR:1','LED_SERIES_RESISTOR:1',#15692,#15696,
'LED_SERIES_RESISTOR:1') ;
#460 = NEXT_ASSEMBLY_USAGE_OCCURRENCE('THERMAL_FUSE_CUTOUT_BLOCK:1',
'THERMAL_FUSE_CUTOUT_BLOCK:1','THERMAL_FUSE_CUTOUT_BLOCK:1',#15692,#15697,
'THERMAL_FUSE_CUTOUT_BLOCK:1') ;
#461 = NEXT_ASSEMBLY_USAGE_OCCURRENCE('THERMAL_FUSE_ELEMENT:1',
'THERMAL_FUSE_ELEMENT:1','THERMAL_FUSE_ELEMENT:1',#15692,#15698,
'THERMAL_FUSE_ELEMENT:1') ;
#462 = NEXT_ASSEMBLY_USAGE_OCCURRENCE('MAINS_CORD_STUB:1',
'MAINS_CORD_STUB:1','MAINS_CORD_STUB:1',#15692,#15699,
'MAINS_CORD_STUB:1') ;
#463 = NEXT_ASSEMBLY_USAGE_OCCURRENCE('RETAINER_SCREW_M3x8:1',
'RETAINER_SCREW_M3x8:1','RETAINER_SCREW_M3x8:1',#15700,#15701,
'RETAINER_SCREW_M3x8:1') ;
#464 = NEXT_ASSEMBLY_USAGE_OCCURRENCE('RETAINER_SCREW_M3x8:2',
'RETAINER_SCREW_M3x8:2','RETAINER_SCREW_M3x8:2',#15700,#15701,
'RETAINER_SCREW_M3x8:2') ;
#465 = NEXT_ASSEMBLY_USAGE_OCCURRENCE('MOUNTING_SCREW_M3x8:1',
'MOUNTING_SCREW_M3x8:1','MOUNTING_SCREW_M3x8:1',#15700,#15702,
'MOUNTING_SCREW_M3x8:1') ;
#466 = NEXT_ASSEMBLY_USAGE_OCCURRENCE('MOUNTING_SCREW_M3x8:2',
'MOUNTING_SCREW_M3x8:2','MOUNTING_SCREW_M3x8:2',#15700,#15702,
'MOUNTING_SCREW_M3x8:2') ;
#467 = NEXT_ASSEMBLY_USAGE_OCCURRENCE('CONTROL_HOUSING_UNIT:1',
'CONTROL_HOUSING_UNIT:1','CONTROL_HOUSING_UNIT:1',#15661,#15662,
'CONTROL_HOUSING_UNIT:1') ;
#468 = NEXT_ASSEMBLY_USAGE_OCCURRENCE('CONNECTOR_UNIT:1',
'CONNECTOR_UNIT:1','CONNECTOR_UNIT:1',#15661,#15665,'CONNECTOR_UNIT:1') ;
#469 = NEXT_ASSEMBLY_USAGE_OCCURRENCE('THERMAL_SENSING_UNIT:1',
'THERMAL_SENSING_UNIT:1','THERMAL_SENSING_UNIT:1',#15661,#15670,
'THERMAL_SENSING_UNIT:1') ;
#470 = NEXT_ASSEMBLY_USAGE_OCCURRENCE('SWITCH_MECHANISM_UNIT:1',
'SWITCH_MECHANISM_UNIT:1','SWITCH_MECHANISM_UNIT:1',#15661,#15680,
'SWITCH_MECHANISM_UNIT:1') ;
#471 = NEXT_ASSEMBLY_USAGE_OCCURRENCE('ELECTRICAL_UNIT:1',
'ELECTRICAL_UNIT:1','ELECTRICAL_UNIT:1',#15661,#15692,
'ELECTRICAL_UNIT:1') ;
#472 = NEXT_ASSEMBLY_USAGE_OCCURRENCE('FASTENERS:1','FASTENERS:1',
'FASTENERS:1',#15661,#15700,'FASTENERS:1') ;
#473 = SHAPE_REPRESENTATION_RELATIONSHIP('SRR','None',#15620,#508) ;
#474 = SHAPE_REPRESENTATION_RELATIONSHIP('SRR','None',#15621,#509) ;
#475 = SHAPE_REPRESENTATION_RELATIONSHIP('SRR','None',#15623,#510) ;
#476 = SHAPE_REPRESENTATION_RELATIONSHIP('SRR','None',#15624,#511) ;
#477 = SHAPE_REPRESENTATION_RELATIONSHIP('SRR','None',#15625,#512) ;
#478 = SHAPE_REPRESENTATION_RELATIONSHIP('SRR','None',#15626,#513) ;
#479 = SHAPE_REPRESENTATION_RELATIONSHIP('SRR','None',#15628,#514) ;
#480 = SHAPE_REPRESENTATION_RELATIONSHIP('SRR','None',#15629,#515) ;
#481 = SHAPE_REPRESENTATION_RELATIONSHIP('SRR','None',#15630,#516) ;
#482 = SHAPE_REPRESENTATION_RELATIONSHIP('SRR','None',#15631,#517) ;
#483 = SHAPE_REPRESENTATION_RELATIONSHIP('SRR','None',#15632,#518) ;
#484 = SHAPE_REPRESENTATION_RELATIONSHIP('SRR','None',#15633,#519) ;
#485 = SHAPE_REPRESENTATION_RELATIONSHIP('SRR','None',#15634,#520) ;
#486 = SHAPE_REPRESENTATION_RELATIONSHIP('SRR','None',#15635,#521) ;
#487 = SHAPE_REPRESENTATION_RELATIONSHIP('SRR','None',#15636,#522) ;
#488 = SHAPE_REPRESENTATION_RELATIONSHIP('SRR','None',#15638,#523) ;
#489 = SHAPE_REPRESENTATION_RELATIONSHIP('SRR','None',#15639,#524) ;
#490 = SHAPE_REPRESENTATION_RELATIONSHIP('SRR','None',#15640,#525) ;
#491 = SHAPE_REPRESENTATION_RELATIONSHIP('SRR','None',#15641,#526) ;
#492 = SHAPE_REPRESENTATION_RELATIONSHIP('SRR','None',#15642,#527) ;
#493 = SHAPE_REPRESENTATION_RELATIONSHIP('SRR','None',#15643,#528) ;
#494 = SHAPE_REPRESENTATION_RELATIONSHIP('SRR','None',#15644,#529) ;
#495 = SHAPE_REPRESENTATION_RELATIONSHIP('SRR','None',#15645,#530) ;
#496 = SHAPE_REPRESENTATION_RELATIONSHIP('SRR','None',#15646,#531) ;
#497 = SHAPE_REPRESENTATION_RELATIONSHIP('SRR','None',#15647,#532) ;
#498 = SHAPE_REPRESENTATION_RELATIONSHIP('SRR','None',#15648,#533) ;
#499 = SHAPE_REPRESENTATION_RELATIONSHIP('SRR','None',#15650,#534) ;
#500 = SHAPE_REPRESENTATION_RELATIONSHIP('SRR','None',#15651,#535) ;
#501 = SHAPE_REPRESENTATION_RELATIONSHIP('SRR','None',#15652,#536) ;
#502 = SHAPE_REPRESENTATION_RELATIONSHIP('SRR','None',#15653,#537) ;
#503 = SHAPE_REPRESENTATION_RELATIONSHIP('SRR','None',#15654,#538) ;
#504 = SHAPE_REPRESENTATION_RELATIONSHIP('SRR','None',#15655,#539) ;
#505 = SHAPE_REPRESENTATION_RELATIONSHIP('SRR','None',#15656,#540) ;
#506 = SHAPE_REPRESENTATION_RELATIONSHIP('SRR','None',#15658,#541) ;
#507 = SHAPE_REPRESENTATION_RELATIONSHIP('SRR','None',#15659,#542) ;
#508 = ADVANCED_BREP_SHAPE_REPRESENTATION('',(#585),#15444) ;
#509 = ADVANCED_BREP_SHAPE_REPRESENTATION('',(#586),#15445) ;
#510 = ADVANCED_BREP_SHAPE_REPRESENTATION('',(#587),#15447) ;
#511 = ADVANCED_BREP_SHAPE_REPRESENTATION('',(#588),#15448) ;
#512 = ADVANCED_BREP_SHAPE_REPRESENTATION('',(#589),#15449) ;
#513 = ADVANCED_BREP_SHAPE_REPRESENTATION('',(#590),#15450) ;
#514 = ADVANCED_BREP_SHAPE_REPRESENTATION('',(#591),#15452) ;
#515 = ADVANCED_BREP_SHAPE_REPRESENTATION('',(#592),#15453) ;
#516 = ADVANCED_BREP_SHAPE_REPRESENTATION('',(#593),#15454) ;
#517 = ADVANCED_BREP_SHAPE_REPRESENTATION('',(#594),#15455) ;
#518 = ADVANCED_BREP_SHAPE_REPRESENTATION('',(#191),#15456) ;
#519 = ADVANCED_BREP_SHAPE_REPRESENTATION('',(#595),#15457) ;
#520 = ADVANCED_BREP_SHAPE_REPRESENTATION('',(#596),#15458) ;
#521 = ADVANCED_BREP_SHAPE_REPRESENTATION('',(#597),#15459) ;
#522 = ADVANCED_BREP_SHAPE_REPRESENTATION('',(#598),#15460) ;
#523 = ADVANCED_BREP_SHAPE_REPRESENTATION('',(#599),#15462) ;
#524 = ADVANCED_BREP_SHAPE_REPRESENTATION('',(#600),#15463) ;
#525 = ADVANCED_BREP_SHAPE_REPRESENTATION('',(#601),#15464) ;
#526 = ADVANCED_BREP_SHAPE_REPRESENTATION('',(#602),#15465) ;
#527 = ADVANCED_BREP_SHAPE_REPRESENTATION('',(#603),#15466) ;
#528 = ADVANCED_BREP_SHAPE_REPRESENTATION('',(#604),#15467) ;
#529 = ADVANCED_BREP_SHAPE_REPRESENTATION('',(#605),#15468) ;
#530 = ADVANCED_BREP_SHAPE_REPRESENTATION('',(#606,#607),#15469) ;
#531 = ADVANCED_BREP_SHAPE_REPRESENTATION('',(#608),#15470) ;
#532 = ADVANCED_BREP_SHAPE_REPRESENTATION('',(#609),#15471) ;
#533 = ADVANCED_BREP_SHAPE_REPRESENTATION('',(#610),#15472) ;
#534 = ADVANCED_BREP_SHAPE_REPRESENTATION('',(#611),#15474) ;
#535 = ADVANCED_BREP_SHAPE_REPRESENTATION('',(#612),#15475) ;
#536 = ADVANCED_BREP_SHAPE_REPRESENTATION('',(#613,#614,#615),#15476) ;
#537 = ADVANCED_BREP_SHAPE_REPRESENTATION('',(#616,#617,#618),#15477) ;
#538 = ADVANCED_BREP_SHAPE_REPRESENTATION('',(#619),#15478) ;
#539 = ADVANCED_BREP_SHAPE_REPRESENTATION('',(#620,#621,#622),#15479) ;
#540 = ADVANCED_BREP_SHAPE_REPRESENTATION('',(#623),#15480) ;
#541 = ADVANCED_BREP_SHAPE_REPRESENTATION('',(#624),#15482) ;
#542 = ADVANCED_BREP_SHAPE_REPRESENTATION('',(#625),#15483) ;
#543 = STYLED_ITEM('',(#15833),#585) ;
#544 = STYLED_ITEM('',(#15833),#586) ;
#545 = STYLED_ITEM('',(#15833),#587) ;
#546 = STYLED_ITEM('',(#15834),#588) ;
#547 = STYLED_ITEM('',(#15834),#589) ;
#548 = STYLED_ITEM('',(#15834),#590) ;
#549 = STYLED_ITEM('',(#15834),#591) ;
#550 = STYLED_ITEM('',(#15835),#592) ;
#551 = STYLED_ITEM('',(#15832),#593) ;
#552 = STYLED_ITEM('',(#15836),#594) ;
#553 = STYLED_ITEM('',(#15836),#191) ;
#554 = STYLED_ITEM('',(#15837),#595) ;
#555 = STYLED_ITEM('',(#15834),#596) ;
#556 = STYLED_ITEM('',(#15835),#597) ;
#557 = STYLED_ITEM('',(#15832),#598) ;
#558 = STYLED_ITEM('',(#15833),#599) ;
#559 = STYLED_ITEM('',(#15832),#600) ;
#560 = STYLED_ITEM('',(#15832),#601) ;
#561 = STYLED_ITEM('',(#15833),#602) ;
#562 = STYLED_ITEM('',(#15838),#603) ;
#563 = STYLED_ITEM('',(#15832),#604) ;
#564 = STYLED_ITEM('',(#15834),#605) ;
#565 = STYLED_ITEM('',(#15834),#606) ;
#566 = STYLED_ITEM('',(#15834),#607) ;
#567 = STYLED_ITEM('',(#15834),#608) ;
#568 = STYLED_ITEM('',(#15839),#609) ;
#569 = STYLED_ITEM('',(#15832),#610) ;
#570 = STYLED_ITEM('',(#15834),#611) ;
#571 = STYLED_ITEM('',(#15840),#612) ;
#572 = STYLED_ITEM('',(#15841),#613) ;
#573 = STYLED_ITEM('',(#15842),#614) ;
#574 = STYLED_ITEM('',(#15842),#615) ;
#575 = STYLED_ITEM('',(#15833),#616) ;
#576 = STYLED_ITEM('',(#15842),#617) ;
#577 = STYLED_ITEM('',(#15842),#618) ;
#578 = STYLED_ITEM('',(#15833),#619) ;
#579 = STYLED_ITEM('',(#15835),#620) ;
#580 = STYLED_ITEM('',(#15842),#621) ;
#581 = STYLED_ITEM('',(#15842),#622) ;
#582 = STYLED_ITEM('',(#15843),#623) ;
#583 = STYLED_ITEM('',(#15832),#624) ;
#584 = STYLED_ITEM('',(#15832),#625) ;
#585 = MANIFOLD_SOLID_BREP('CONTROL_HOUSING_BODY',#8252) ;
#586 = MANIFOLD_SOLID_BREP('BASE_STATION_CORD_RETAINER',#8253) ;
#587 = MANIFOLD_SOLID_BREP('STANDARD_3PIN_STRIX_CONNECTOR_BASE',#8254) ;
#588 = MANIFOLD_SOLID_BREP('EARTH_CONTACT_RING',#8255) ;
#589 = MANIFOLD_SOLID_BREP('LIVE_CONTACT_RING',#8256) ;
#590 = MANIFOLD_SOLID_BREP('NEUTRAL_CENTRE_PIN',#8257) ;
#591 = MANIFOLD_SOLID_BREP('STEAM_DISC_HOLDER_CUP',#8258) ;
#592 = MANIFOLD_SOLID_BREP('BIMETALLIC_THERMOSTATIC_DISC_UNIT',#8259) ;
#593 = MANIFOLD_SOLID_BREP('STEAM_DISC_PUSH_ROD',#8260) ;
#594 = MANIFOLD_SOLID_BREP('STEAM_PORT_DEFLECTOR_CAP',#8261) ;
#595 = MANIFOLD_SOLID_BREP('STEAM_SEAL_GROMMET',#8265) ;
#596 = MANIFOLD_SOLID_BREP('DRY_BOIL_DISC_HOLDER',#8266) ;
#597 = MANIFOLD_SOLID_BREP('DRY_BOIL_BIMETAL_DISC',#8267) ;
#598 = MANIFOLD_SOLID_BREP('DRY_BOIL_PUSH_ROD',#8268) ;
#599 = MANIFOLD_SOLID_BREP('AUTO_OFF_LATCH_TRIP_LEVER',#8269) ;
#600 = MANIFOLD_SOLID_BREP('TRIP_LEVER_PIVOT_PIN',#8270) ;
#601 = MANIFOLD_SOLID_BREP('TRIP_LEVER_RETURN_SPRING',#8271) ;
#602 = MANIFOLD_SOLID_BREP('PUSH_BUTTON_STEM',#8272) ;
#603 = MANIFOLD_SOLID_BREP('PUSH_BUTTON_CAP',#8273) ;
#604 = MANIFOLD_SOLID_BREP('BUTTON_RETURN_SPRING',#8274) ;
#605 = MANIFOLD_SOLID_BREP('MOVING_CONTACT_ARM',#8275) ;
#606 = MANIFOLD_SOLID_BREP('CONTACT_ANCHOR_POST',#8276) ;
#607 = MANIFOLD_SOLID_BREP('CONTACT_ANCHOR_POST',#8277) ;
#608 = MANIFOLD_SOLID_BREP('FIXED_CONTACT_POST',#8278) ;
#609 = MANIFOLD_SOLID_BREP('CONTACT_RIVET_SILVER',#8279) ;
#610 = MANIFOLD_SOLID_BREP('CONTACT_PRESSURE_SPRING',#8280) ;
#611 = MANIFOLD_SOLID_BREP('ELECTRICAL_TERMINAL_CONTACT_PIN',#8281) ;
#612 = MANIFOLD_SOLID_BREP('INDICATOR_LED_LIGHT_HOUSING',#8282) ;
#613 = MANIFOLD_SOLID_BREP('LED_BODY',#8283) ;
#614 = MANIFOLD_SOLID_BREP('LED_LEADS',#8284) ;
#615 = MANIFOLD_SOLID_BREP('LED_LEADS',#8285) ;
#616 = MANIFOLD_SOLID_BREP('RESISTOR_BODY',#8286) ;
#617 = MANIFOLD_SOLID_BREP('RESISTOR_LEADS',#8287) ;
#618 = MANIFOLD_SOLID_BREP('RESISTOR_LEADS',#8288) ;
#619 = MANIFOLD_SOLID_BREP('THERMAL_FUSE_CUTOUT_BLOCK',#8289) ;
#620 = MANIFOLD_SOLID_BREP('FUSE_BODY',#8290) ;
#621 = MANIFOLD_SOLID_BREP('FUSE_LEADS',#8291) ;
#622 = MANIFOLD_SOLID_BREP('FUSE_LEADS',#8292) ;
#623 = MANIFOLD_SOLID_BREP('MAINS_CORD_STUB',#8293) ;
#624 = MANIFOLD_SOLID_BREP('RETAINER_SCREW_M3x8',#8294) ;
#625 = MANIFOLD_SOLID_BREP('MOUNTING_SCREW_M3x8',#8295) ;
#626 = CYLINDRICAL_SURFACE('',#8695,0.155) ;
#627 = CYLINDRICAL_SURFACE('',#8699,0.155) ;
#628 = CYLINDRICAL_SURFACE('',#8703,0.17) ;
#629 = CYLINDRICAL_SURFACE('',#8711,0.17) ;
#630 = CYLINDRICAL_SURFACE('',#8719,0.14) ;
#631 = CYLINDRICAL_SURFACE('',#8722,0.4) ;
#632 = CYLINDRICAL_SURFACE('',#8726,0.8) ;
#633 = CYLINDRICAL_SURFACE('',#8729,1.) ;
#634 = CYLINDRICAL_SURFACE('',#8732,0.21) ;
#635 = CYLINDRICAL_SURFACE('',#8735,0.4) ;
#636 = CYLINDRICAL_SURFACE('',#8739,0.13) ;
#637 = CYLINDRICAL_SURFACE('',#8742,0.13) ;
#638 = CYLINDRICAL_SURFACE('',#8755,1.31) ;
#639 = CYLINDRICAL_SURFACE('',#8765,0.295) ;
#640 = CYLINDRICAL_SURFACE('',#8771,0.295) ;
#641 = CYLINDRICAL_SURFACE('',#8776,0.17) ;
#642 = CYLINDRICAL_SURFACE('',#8778,0.295) ;
#643 = CYLINDRICAL_SURFACE('',#8781,0.295) ;
#644 = CYLINDRICAL_SURFACE('',#8789,0.17) ;
#645 = CYLINDRICAL_SURFACE('',#8791,0.31) ;
#646 = CYLINDRICAL_SURFACE('',#8800,0.26) ;
#647 = CYLINDRICAL_SURFACE('',#8819,0.69) ;
#648 = CYLINDRICAL_SURFACE('',#8822,0.81) ;
#649 = CYLINDRICAL_SURFACE('',#8828,1.09) ;
#650 = CYLINDRICAL_SURFACE('',#8830,1.21) ;
#651 = CYLINDRICAL_SURFACE('',#8836,1.3) ;
#652 = CYLINDRICAL_SURFACE('',#8841,1.1) ;
#653 = CYLINDRICAL_SURFACE('',#8844,1.2) ;
#654 = CYLINDRICAL_SURFACE('',#8850,0.7) ;
#655 = CYLINDRICAL_SURFACE('',#8853,0.8) ;
#656 = CYLINDRICAL_SURFACE('',#8862,0.25) ;
#657 = CYLINDRICAL_SURFACE('',#8871,0.13) ;
#658 = CYLINDRICAL_SURFACE('',#8874,0.7) ;
#659 = CYLINDRICAL_SURFACE('',#8879,0.8) ;
#660 = CYLINDRICAL_SURFACE('',#8884,0.2) ;
#661 = CYLINDRICAL_SURFACE('',#8888,0.69) ;
#662 = CYLINDRICAL_SURFACE('',#8894,0.12) ;
#663 = CYLINDRICAL_SURFACE('',#8912,0.13) ;
#664 = CYLINDRICAL_SURFACE('',#8918,0.41) ;
#665 = CYLINDRICAL_SURFACE('',#8922,0.81) ;
#666 = CYLINDRICAL_SURFACE('',#8929,1.2) ;
#667 = CYLINDRICAL_SURFACE('',#8938,0.3) ;
#668 = CYLINDRICAL_SURFACE('',#8940,0.3) ;
#669 = CYLINDRICAL_SURFACE('',#8944,0.4) ;
#670 = CYLINDRICAL_SURFACE('',#8946,0.4) ;
#671 = CYLINDRICAL_SURFACE('',#8953,0.4) ;
#672 = CYLINDRICAL_SURFACE('',#8955,0.4) ;
#673 = CYLINDRICAL_SURFACE('',#8958,0.3) ;
#674 = CYLINDRICAL_SURFACE('',#8961,0.3) ;
#675 = CYLINDRICAL_SURFACE('',#8968,0.4) ;
#676 = CYLINDRICAL_SURFACE('',#8971,0.45) ;
#677 = CYLINDRICAL_SURFACE('',#8977,0.13) ;
#678 = CYLINDRICAL_SURFACE('',#8980,0.71) ;
#679 = CYLINDRICAL_SURFACE('',#8985,0.85) ;
#680 = CYLINDRICAL_SURFACE('',#8990,0.7) ;
#681 = CYLINDRICAL_SURFACE('',#8996,0.12) ;
#682 = CYLINDRICAL_SURFACE('',#9012,0.13) ;
#683 = CYLINDRICAL_SURFACE('',#9023,0.13) ;
#684 = CYLINDRICAL_SURFACE('',#9025,0.3) ;
#685 = CYLINDRICAL_SURFACE('',#9027,0.3) ;
#686 = CYLINDRICAL_SURFACE('',#9038,0.2) ;
#687 = CYLINDRICAL_SURFACE('',#9041,0.125) ;
#688 = CYLINDRICAL_SURFACE('',#9202,0.025) ;
#689 = CYLINDRICAL_SURFACE('',#9208,0.025) ;
#690 = CYLINDRICAL_SURFACE('',#9211,0.025) ;
#691 = CYLINDRICAL_SURFACE('',#9213,0.025) ;
#692 = CYLINDRICAL_SURFACE('',#9215,0.025) ;
#693 = CYLINDRICAL_SURFACE('',#9217,0.025) ;
#694 = CYLINDRICAL_SURFACE('',#9220,0.025) ;
#695 = CYLINDRICAL_SURFACE('',#9224,0.025) ;
#696 = CYLINDRICAL_SURFACE('',#9227,0.025) ;
#697 = CYLINDRICAL_SURFACE('',#9231,0.025) ;
#698 = CYLINDRICAL_SURFACE('',#9234,0.025) ;
#699 = CYLINDRICAL_SURFACE('',#9236,0.025) ;
#700 = CYLINDRICAL_SURFACE('',#9238,0.025) ;
#701 = CYLINDRICAL_SURFACE('',#9240,0.025) ;
#702 = CYLINDRICAL_SURFACE('',#9243,0.025) ;
#703 = CYLINDRICAL_SURFACE('',#9247,0.025) ;
#704 = CYLINDRICAL_SURFACE('',#9250,0.025) ;
#705 = CYLINDRICAL_SURFACE('',#9254,0.025) ;
#706 = CYLINDRICAL_SURFACE('',#9257,0.025) ;
#707 = CYLINDRICAL_SURFACE('',#9259,0.025) ;
#708 = CYLINDRICAL_SURFACE('',#9261,0.025) ;
#709 = CYLINDRICAL_SURFACE('',#9263,0.025) ;
#710 = CYLINDRICAL_SURFACE('',#9266,0.025) ;
#711 = CYLINDRICAL_SURFACE('',#9270,0.025) ;
#712 = CYLINDRICAL_SURFACE('',#9273,0.025) ;
#713 = CYLINDRICAL_SURFACE('',#9277,0.025) ;
#714 = CYLINDRICAL_SURFACE('',#9280,0.025) ;
#715 = CYLINDRICAL_SURFACE('',#9282,0.025) ;
#716 = CYLINDRICAL_SURFACE('',#9284,0.025) ;
#717 = CYLINDRICAL_SURFACE('',#9286,0.025) ;
#718 = CYLINDRICAL_SURFACE('',#9289,0.025) ;
#719 = CYLINDRICAL_SURFACE('',#9293,0.025) ;
#720 = CYLINDRICAL_SURFACE('',#9296,0.025) ;
#721 = CYLINDRICAL_SURFACE('',#9300,0.025) ;
#722 = CYLINDRICAL_SURFACE('',#9303,0.025) ;
#723 = CYLINDRICAL_SURFACE('',#9305,0.025) ;
#724 = CYLINDRICAL_SURFACE('',#9307,0.025) ;
#725 = CYLINDRICAL_SURFACE('',#9309,0.025) ;
#726 = CYLINDRICAL_SURFACE('',#9312,0.025) ;
#727 = CYLINDRICAL_SURFACE('',#9316,0.025) ;
#728 = CYLINDRICAL_SURFACE('',#9326,0.35) ;
#729 = CYLINDRICAL_SURFACE('',#9327,0.2) ;
#730 = CYLINDRICAL_SURFACE('',#9329,0.2) ;
#731 = CYLINDRICAL_SURFACE('',#9339,0.21) ;
#732 = CYLINDRICAL_SURFACE('',#9443,0.025) ;
#733 = CYLINDRICAL_SURFACE('',#9449,0.025) ;
#734 = CYLINDRICAL_SURFACE('',#9452,0.025) ;
#735 = CYLINDRICAL_SURFACE('',#9454,0.025) ;
#736 = CYLINDRICAL_SURFACE('',#9456,0.025) ;
#737 = CYLINDRICAL_SURFACE('',#9458,0.025) ;
#738 = CYLINDRICAL_SURFACE('',#9461,0.025) ;
#739 = CYLINDRICAL_SURFACE('',#9465,0.025) ;
#740 = CYLINDRICAL_SURFACE('',#9468,0.025) ;
#741 = CYLINDRICAL_SURFACE('',#9472,0.025) ;
#742 = CYLINDRICAL_SURFACE('',#9475,0.025) ;
#743 = CYLINDRICAL_SURFACE('',#9477,0.025) ;
#744 = CYLINDRICAL_SURFACE('',#9479,0.025) ;
#745 = CYLINDRICAL_SURFACE('',#9481,0.025) ;
#746 = CYLINDRICAL_SURFACE('',#9484,0.025) ;
#747 = CYLINDRICAL_SURFACE('',#9488,0.025) ;
#748 = CYLINDRICAL_SURFACE('',#9491,0.025) ;
#749 = CYLINDRICAL_SURFACE('',#9495,0.025) ;
#750 = CYLINDRICAL_SURFACE('',#9498,0.025) ;
#751 = CYLINDRICAL_SURFACE('',#9500,0.025) ;
#752 = CYLINDRICAL_SURFACE('',#9502,0.025) ;
#753 = CYLINDRICAL_SURFACE('',#9504,0.025) ;
#754 = CYLINDRICAL_SURFACE('',#9507,0.025) ;
#755 = CYLINDRICAL_SURFACE('',#9511,0.025) ;
#756 = CYLINDRICAL_SURFACE('',#9515,0.15) ;
#757 = CYLINDRICAL_SURFACE('',#9526,0.15) ;
#758 = CYLINDRICAL_SURFACE('',#9531,0.15) ;
#759 = CYLINDRICAL_SURFACE('',#9537,0.15) ;
#760 = CYLINDRICAL_SURFACE('',#9543,0.15) ;
#761 = CYLINDRICAL_SURFACE('',#9674,0.02) ;
#762 = CYLINDRICAL_SURFACE('',#9680,0.02) ;
#763 = CYLINDRICAL_SURFACE('',#9683,0.02) ;
#764 = CYLINDRICAL_SURFACE('',#9685,0.02) ;
#765 = CYLINDRICAL_SURFACE('',#9687,0.02) ;
#766 = CYLINDRICAL_SURFACE('',#9689,0.02) ;
#767 = CYLINDRICAL_SURFACE('',#9692,0.02) ;
#768 = CYLINDRICAL_SURFACE('',#9696,0.02) ;
#769 = CYLINDRICAL_SURFACE('',#9699,0.02) ;
#770 = CYLINDRICAL_SURFACE('',#9703,0.02) ;
#771 = CYLINDRICAL_SURFACE('',#9706,0.02) ;
#772 = CYLINDRICAL_SURFACE('',#9708,0.02) ;
#773 = CYLINDRICAL_SURFACE('',#9710,0.02) ;
#774 = CYLINDRICAL_SURFACE('',#9712,0.02) ;
#775 = CYLINDRICAL_SURFACE('',#9715,0.02) ;
#776 = CYLINDRICAL_SURFACE('',#9719,0.02) ;
#777 = CYLINDRICAL_SURFACE('',#9722,0.02) ;
#778 = CYLINDRICAL_SURFACE('',#9726,0.02) ;
#779 = CYLINDRICAL_SURFACE('',#9729,0.02) ;
#780 = CYLINDRICAL_SURFACE('',#9731,0.02) ;
#781 = CYLINDRICAL_SURFACE('',#9733,0.02) ;
#782 = CYLINDRICAL_SURFACE('',#9735,0.02) ;
#783 = CYLINDRICAL_SURFACE('',#9738,0.02) ;
#784 = CYLINDRICAL_SURFACE('',#9742,0.02) ;
#785 = CYLINDRICAL_SURFACE('',#9745,0.02) ;
#786 = CYLINDRICAL_SURFACE('',#9749,0.02) ;
#787 = CYLINDRICAL_SURFACE('',#9752,0.02) ;
#788 = CYLINDRICAL_SURFACE('',#9754,0.02) ;
#789 = CYLINDRICAL_SURFACE('',#9756,0.02) ;
#790 = CYLINDRICAL_SURFACE('',#9758,0.02) ;
#791 = CYLINDRICAL_SURFACE('',#9761,0.02) ;
#792 = CYLINDRICAL_SURFACE('',#9765,0.02) ;
#793 = CYLINDRICAL_SURFACE('',#9781,0.08) ;
#794 = CYLINDRICAL_SURFACE('',#9801,0.16) ;
#795 = CYLINDRICAL_SURFACE('',#9815,0.15) ;
#796 = CYLINDRICAL_SURFACE('',#9818,0.025) ;
#797 = CYLINDRICAL_SURFACE('',#9823,0.025) ;
#798 = CYLINDRICAL_SURFACE('',#9829,0.115) ;
#799 = CYLINDRICAL_SURFACE('',#9834,0.025) ;
#800 = CYLINDRICAL_SURFACE('',#9839,0.025) ;
#801 = CYLINDRICAL_SURFACE('',#9856,0.21) ;
#802 = CYLINDRICAL_SURFACE('',#9864,0.2) ;
#803 = CYLINDRICAL_SURFACE('',#9869,0.04) ;
#804 = CYLINDRICAL_SURFACE('',#9874,0.04) ;
#805 = CYLINDRICAL_SURFACE('',#9880,0.29) ;
#806 = CYLINDRICAL_SURFACE('',#9896,0.15) ;
#807 = CYLINDRICAL_SURFACE('',#9900,0.275) ;
#808 = CYLINDRICAL_SURFACE('',#9906,0.15) ;
#809 = CYLINDRICAL_SURFACE('',#9910,0.275) ;
#810 = FACE_BOUND('',#1871,.T.) ;
#811 = FACE_BOUND('',#1872,.T.) ;
#812 = FACE_BOUND('',#1873,.T.) ;
#813 = FACE_BOUND('',#1874,.T.) ;
#814 = FACE_BOUND('',#1875,.T.) ;
#815 = FACE_BOUND('',#1876,.T.) ;
#816 = FACE_BOUND('',#1883,.T.) ;
#817 = FACE_BOUND('',#1890,.T.) ;
#818 = FACE_BOUND('',#1898,.T.) ;
#819 = FACE_BOUND('',#1903,.T.) ;
#820 = FACE_BOUND('',#1907,.T.) ;
#821 = FACE_BOUND('',#1913,.T.) ;
#822 = FACE_BOUND('',#1916,.T.) ;
#823 = FACE_BOUND('',#1920,.T.) ;
#824 = FACE_BOUND('',#1923,.T.) ;
#825 = FACE_BOUND('',#1930,.T.) ;
#826 = FACE_BOUND('',#1932,.T.) ;
#827 = FACE_BOUND('',#1933,.T.) ;
#828 = FACE_BOUND('',#1934,.T.) ;
#829 = FACE_BOUND('',#1935,.T.) ;
#830 = FACE_BOUND('',#1936,.T.) ;
#831 = FACE_BOUND('',#1941,.T.) ;
#832 = FACE_BOUND('',#1944,.T.) ;
#833 = FACE_BOUND('',#1950,.T.) ;
#834 = FACE_BOUND('',#1957,.T.) ;
#835 = FACE_BOUND('',#1958,.T.) ;
#836 = FACE_BOUND('',#1961,.T.) ;
#837 = FACE_BOUND('',#1982,.T.) ;
#838 = FACE_BOUND('',#1984,.T.) ;
#839 = FACE_BOUND('',#1988,.T.) ;
#840 = FACE_BOUND('',#1990,.T.) ;
#841 = FACE_BOUND('',#1993,.T.) ;
#842 = FACE_BOUND('',#1995,.T.) ;
#843 = FACE_BOUND('',#1996,.T.) ;
#844 = FACE_BOUND('',#1997,.T.) ;
#845 = FACE_BOUND('',#2001,.T.) ;
#846 = FACE_BOUND('',#2003,.T.) ;
#847 = FACE_BOUND('',#2007,.T.) ;
#848 = FACE_BOUND('',#2009,.T.) ;
#849 = FACE_BOUND('',#2016,.T.) ;
#850 = FACE_BOUND('',#2019,.T.) ;
#851 = FACE_BOUND('',#2021,.T.) ;
#852 = FACE_BOUND('',#2027,.T.) ;
#853 = FACE_BOUND('',#2043,.T.) ;
#854 = FACE_BOUND('',#2045,.T.) ;
#855 = FACE_BOUND('',#2047,.T.) ;
#856 = FACE_BOUND('',#2048,.T.) ;
#857 = FACE_BOUND('',#2050,.T.) ;
#858 = FACE_BOUND('',#2052,.T.) ;
#859 = FACE_BOUND('',#2058,.T.) ;
#860 = FACE_BOUND('',#2062,.T.) ;
#861 = FACE_BOUND('',#2073,.T.) ;
#862 = FACE_BOUND('',#2075,.T.) ;
#863 = FACE_BOUND('',#2079,.T.) ;
#864 = FACE_BOUND('',#2082,.T.) ;
#865 = FACE_BOUND('',#2084,.T.) ;
#866 = FACE_BOUND('',#2096,.T.) ;
#867 = FACE_BOUND('',#2102,.T.) ;
#868 = FACE_BOUND('',#2105,.T.) ;
#869 = FACE_BOUND('',#2107,.T.) ;
#870 = FACE_BOUND('',#2110,.T.) ;
#871 = FACE_BOUND('',#2197,.T.) ;
#872 = FACE_BOUND('',#2199,.T.) ;
#873 = FACE_BOUND('',#2213,.T.) ;
#874 = FACE_BOUND('',#2215,.T.) ;
#875 = FACE_BOUND('',#2272,.T.) ;
#876 = FACE_BOUND('',#2357,.T.) ;
#877 = FACE_BOUND('',#2360,.T.) ;
#878 = FACE_BOUND('',#2373,.T.) ;
#879 = FACE_BOUND('',#2379,.T.) ;
#880 = FACE_BOUND('',#2382,.T.) ;
#881 = FACE_BOUND('',#2413,.T.) ;
#882 = FACE_BOUND('',#2415,.T.) ;
#883 = FACE_BOUND('',#2433,.T.) ;
#884 = FACE_BOUND('',#2439,.T.) ;
#885 = CIRCLE('',#8691,0.4) ;
#886 = CIRCLE('',#8692,0.4) ;
#887 = CIRCLE('',#8693,1.31) ;
#888 = CIRCLE('',#8694,1.) ;
#889 = CIRCLE('',#8696,0.155) ;
#890 = CIRCLE('',#8697,0.155) ;
#891 = CIRCLE('',#8700,0.155) ;
#892 = CIRCLE('',#8701,0.155) ;
#893 = CIRCLE('',#8704,0.17) ;
#894 = CIRCLE('',#8705,0.17) ;
#895 = CIRCLE('',#8712,0.17) ;
#896 = CIRCLE('',#8713,0.17) ;
#897 = CIRCLE('',#8720,0.14) ;
#898 = CIRCLE('',#8721,0.14) ;
#899 = CIRCLE('',#8723,0.4) ;
#900 = CIRCLE('',#8727,0.8) ;
#901 = CIRCLE('',#8728,0.8) ;
#902 = CIRCLE('',#8730,1.) ;
#903 = CIRCLE('',#8733,0.21) ;
#904 = CIRCLE('',#8734,0.21) ;
#905 = CIRCLE('',#8736,0.4) ;
#906 = CIRCLE('',#8740,0.13) ;
#907 = CIRCLE('',#8741,0.13) ;
#908 = CIRCLE('',#8743,0.13) ;
#909 = CIRCLE('',#8744,0.13) ;
#910 = CIRCLE('',#8756,1.31) ;
#911 = CIRCLE('',#8766,0.295) ;
#912 = CIRCLE('',#8767,0.295) ;
#913 = CIRCLE('',#8769,0.295) ;
#914 = CIRCLE('',#8770,0.17) ;
#915 = CIRCLE('',#8772,0.295) ;
#916 = CIRCLE('',#8774,0.31) ;
#917 = CIRCLE('',#8777,0.17) ;
#918 = CIRCLE('',#8779,0.295) ;
#919 = CIRCLE('',#8780,0.295) ;
#920 = CIRCLE('',#8782,0.295) ;
#921 = CIRCLE('',#8783,0.295) ;
#922 = CIRCLE('',#8785,0.17) ;
#923 = CIRCLE('',#8790,0.17) ;
#924 = CIRCLE('',#8792,0.31) ;
#925 = CIRCLE('',#8801,0.26) ;
#926 = CIRCLE('',#8802,0.26) ;
#927 = CIRCLE('',#8820,0.69) ;
#928 = CIRCLE('',#8821,0.69) ;
#929 = CIRCLE('',#8823,0.81) ;
#930 = CIRCLE('',#8824,0.81) ;
#931 = CIRCLE('',#8827,1.09) ;
#932 = CIRCLE('',#8829,1.09) ;
#933 = CIRCLE('',#8831,1.21) ;
#934 = CIRCLE('',#8832,1.21) ;
#935 = CIRCLE('',#8835,1.3) ;
#936 = CIRCLE('',#8837,1.3) ;
#937 = CIRCLE('',#8842,1.1) ;
#938 = CIRCLE('',#8843,1.1) ;
#939 = CIRCLE('',#8845,1.2) ;
#940 = CIRCLE('',#8846,1.2) ;
#941 = CIRCLE('',#8851,0.7) ;
#942 = CIRCLE('',#8852,0.7) ;
#943 = CIRCLE('',#8854,0.8) ;
#944 = CIRCLE('',#8855,0.8) ;
#945 = CIRCLE('',#8860,0.25) ;
#946 = CIRCLE('',#8861,0.25) ;
#947 = CIRCLE('',#8863,0.25) ;
#948 = CIRCLE('',#8872,0.13) ;
#949 = CIRCLE('',#8873,0.13) ;
#950 = CIRCLE('',#8875,0.7) ;
#951 = CIRCLE('',#8876,0.7) ;
#952 = CIRCLE('',#8878,0.8) ;
#953 = CIRCLE('',#8880,0.8) ;
#954 = CIRCLE('',#8885,0.2) ;
#955 = CIRCLE('',#8886,0.2) ;
#956 = CIRCLE('',#8889,0.69) ;
#957 = CIRCLE('',#8890,0.69) ;
#958 = CIRCLE('',#8895,0.12) ;
#959 = CIRCLE('',#8896,0.12) ;
#960 = CIRCLE('',#8902,1.2) ;
#961 = CIRCLE('',#8905,1.2) ;
#962 = CIRCLE('',#8907,0.81) ;
#963 = CIRCLE('',#8909,0.81) ;
#964 = CIRCLE('',#8913,0.13) ;
#965 = CIRCLE('',#8914,0.13) ;
#966 = CIRCLE('',#8916,0.81) ;
#967 = CIRCLE('',#8917,0.41) ;
#968 = CIRCLE('',#8919,0.41) ;
#969 = CIRCLE('',#8920,0.41) ;
#970 = CIRCLE('',#8921,0.41) ;
#971 = CIRCLE('',#8923,0.81) ;
#972 = CIRCLE('',#8924,0.81) ;
#973 = CIRCLE('',#8925,0.81) ;
#974 = CIRCLE('',#8928,1.2) ;
#975 = CIRCLE('',#8930,1.2) ;
#976 = CIRCLE('',#8934,0.3) ;
#977 = CIRCLE('',#8936,0.3) ;
#978 = CIRCLE('',#8937,0.3) ;
#979 = CIRCLE('',#8942,0.4) ;
#980 = CIRCLE('',#8943,0.3) ;
#981 = CIRCLE('',#8945,0.4) ;
#982 = CIRCLE('',#8948,0.4) ;
#983 = CIRCLE('',#8949,0.4) ;
#984 = CIRCLE('',#8951,0.4) ;
#985 = CIRCLE('',#8952,0.3) ;
#986 = CIRCLE('',#8954,0.4) ;
#987 = CIRCLE('',#8956,0.4) ;
#988 = CIRCLE('',#8957,0.4) ;
#989 = CIRCLE('',#8959,0.3) ;
#990 = CIRCLE('',#8960,0.3) ;
#991 = CIRCLE('',#8962,0.3) ;
#992 = CIRCLE('',#8963,0.3) ;
#993 = CIRCLE('',#8969,0.4) ;
#994 = CIRCLE('',#8970,0.4) ;
#995 = CIRCLE('',#8972,0.45) ;
#996 = CIRCLE('',#8973,0.45) ;
#997 = CIRCLE('',#8978,0.13) ;
#998 = CIRCLE('',#8979,0.13) ;
#999 = CIRCLE('',#8981,0.71) ;
#1000 = CIRCLE('',#8982,0.71) ;
#1001 = CIRCLE('',#8984,0.85) ;
#1002 = CIRCLE('',#8986,0.85) ;
#1003 = CIRCLE('',#8991,0.7) ;
#1004 = CIRCLE('',#8992,0.7) ;
#1005 = CIRCLE('',#8997,0.12) ;
#1006 = CIRCLE('',#8998,0.12) ;
#1007 = CIRCLE('',#9013,0.13) ;
#1008 = CIRCLE('',#9014,0.13) ;
#1009 = CIRCLE('',#9019,0.3) ;
#1010 = CIRCLE('',#9020,0.3) ;
#1011 = CIRCLE('',#9021,0.13) ;
#1012 = CIRCLE('',#9024,0.13) ;
#1013 = CIRCLE('',#9026,0.3) ;
#1014 = CIRCLE('',#9028,0.3) ;
#1015 = CIRCLE('',#9036,0.2) ;
#1016 = CIRCLE('',#9037,0.125) ;
#1017 = CIRCLE('',#9039,0.2) ;
#1018 = CIRCLE('',#9042,0.125) ;
#1019 = CIRCLE('',#9046,0.025) ;
#1020 = CIRCLE('',#9047,0.025) ;
#1021 = CIRCLE('',#9049,0.025) ;
#1022 = CIRCLE('',#9050,0.025) ;
#1023 = CIRCLE('',#9051,0.025) ;
#1024 = CIRCLE('',#9053,0.025) ;
#1025 = CIRCLE('',#9054,0.025) ;
#1026 = CIRCLE('',#9055,0.025) ;
#1027 = CIRCLE('',#9056,0.025) ;
#1028 = CIRCLE('',#9058,0.025) ;
#1029 = CIRCLE('',#9059,0.025) ;
#1030 = CIRCLE('',#9060,0.025) ;
#1031 = CIRCLE('',#9061,0.025) ;
#1032 = CIRCLE('',#9063,0.025) ;
#1033 = CIRCLE('',#9064,0.025) ;
#1034 = CIRCLE('',#9065,0.025) ;
#1035 = CIRCLE('',#9066,0.025) ;
#1036 = CIRCLE('',#9068,0.025) ;
#1037 = CIRCLE('',#9069,0.025) ;
#1038 = CIRCLE('',#9070,0.025) ;
#1039 = CIRCLE('',#9072,0.025) ;
#1040 = CIRCLE('',#9073,0.025) ;
#1041 = CIRCLE('',#9075,0.025) ;
#1042 = CIRCLE('',#9076,0.025) ;
#1043 = CIRCLE('',#9078,0.025) ;
#1044 = CIRCLE('',#9079,0.025) ;
#1045 = CIRCLE('',#9081,0.025) ;
#1046 = CIRCLE('',#9082,0.025) ;
#1047 = CIRCLE('',#9083,0.025) ;
#1048 = CIRCLE('',#9085,0.025) ;
#1049 = CIRCLE('',#9086,0.025) ;
#1050 = CIRCLE('',#9087,0.025) ;
#1051 = CIRCLE('',#9088,0.025) ;
#1052 = CIRCLE('',#9090,0.025) ;
#1053 = CIRCLE('',#9091,0.025) ;
#1054 = CIRCLE('',#9092,0.025) ;
#1055 = CIRCLE('',#9093,0.025) ;
#1056 = CIRCLE('',#9095,0.025) ;
#1057 = CIRCLE('',#9096,0.025) ;
#1058 = CIRCLE('',#9097,0.025) ;
#1059 = CIRCLE('',#9098,0.025) ;
#1060 = CIRCLE('',#9100,0.025) ;
#1061 = CIRCLE('',#9101,0.025) ;
#1062 = CIRCLE('',#9102,0.025) ;
#1063 = CIRCLE('',#9104,0.025) ;
#1064 = CIRCLE('',#9105,0.025) ;
#1065 = CIRCLE('',#9107,0.025) ;
#1066 = CIRCLE('',#9108,0.025) ;
#1067 = CIRCLE('',#9110,0.025) ;
#1068 = CIRCLE('',#9111,0.025) ;
#1069 = CIRCLE('',#9113,0.025) ;
#1070 = CIRCLE('',#9114,0.025) ;
#1071 = CIRCLE('',#9115,0.025) ;
#1072 = CIRCLE('',#9117,0.025) ;
#1073 = CIRCLE('',#9118,0.025) ;
#1074 = CIRCLE('',#9119,0.025) ;
#1075 = CIRCLE('',#9120,0.025) ;
#1076 = CIRCLE('',#9122,0.025) ;
#1077 = CIRCLE('',#9123,0.025) ;
#1078 = CIRCLE('',#9124,0.025) ;
#1079 = CIRCLE('',#9125,0.025) ;
#1080 = CIRCLE('',#9127,0.025) ;
#1081 = CIRCLE('',#9128,0.025) ;
#1082 = CIRCLE('',#9129,0.025) ;
#1083 = CIRCLE('',#9130,0.025) ;
#1084 = CIRCLE('',#9132,0.025) ;
#1085 = CIRCLE('',#9133,0.025) ;
#1086 = CIRCLE('',#9134,0.025) ;
#1087 = CIRCLE('',#9136,0.025) ;
#1088 = CIRCLE('',#9137,0.025) ;
#1089 = CIRCLE('',#9139,0.025) ;
#1090 = CIRCLE('',#9140,0.025) ;
#1091 = CIRCLE('',#9142,0.025) ;
#1092 = CIRCLE('',#9143,0.025) ;
#1093 = CIRCLE('',#9145,0.025) ;
#1094 = CIRCLE('',#9146,0.025) ;
#1095 = CIRCLE('',#9147,0.025) ;
#1096 = CIRCLE('',#9149,0.025) ;
#1097 = CIRCLE('',#9150,0.025) ;
#1098 = CIRCLE('',#9151,0.025) ;
#1099 = CIRCLE('',#9152,0.025) ;
#1100 = CIRCLE('',#9154,0.025) ;
#1101 = CIRCLE('',#9155,0.025) ;
#1102 = CIRCLE('',#9156,0.025) ;
#1103 = CIRCLE('',#9157,0.025) ;
#1104 = CIRCLE('',#9159,0.025) ;
#1105 = CIRCLE('',#9160,0.025) ;
#1106 = CIRCLE('',#9161,0.025) ;
#1107 = CIRCLE('',#9162,0.025) ;
#1108 = CIRCLE('',#9164,0.025) ;
#1109 = CIRCLE('',#9165,0.025) ;
#1110 = CIRCLE('',#9166,0.025) ;
#1111 = CIRCLE('',#9168,0.025) ;
#1112 = CIRCLE('',#9169,0.025) ;
#1113 = CIRCLE('',#9171,0.025) ;
#1114 = CIRCLE('',#9172,0.025) ;
#1115 = CIRCLE('',#9174,0.025) ;
#1116 = CIRCLE('',#9175,0.025) ;
#1117 = CIRCLE('',#9177,0.025) ;
#1118 = CIRCLE('',#9178,0.025) ;
#1119 = CIRCLE('',#9179,0.025) ;
#1120 = CIRCLE('',#9181,0.025) ;
#1121 = CIRCLE('',#9182,0.025) ;
#1122 = CIRCLE('',#9183,0.025) ;
#1123 = CIRCLE('',#9184,0.025) ;
#1124 = CIRCLE('',#9186,0.025) ;
#1125 = CIRCLE('',#9187,0.025) ;
#1126 = CIRCLE('',#9188,0.025) ;
#1127 = CIRCLE('',#9189,0.025) ;
#1128 = CIRCLE('',#9191,0.025) ;
#1129 = CIRCLE('',#9192,0.025) ;
#1130 = CIRCLE('',#9193,0.025) ;
#1131 = CIRCLE('',#9194,0.025) ;
#1132 = CIRCLE('',#9196,0.025) ;
#1133 = CIRCLE('',#9197,0.025) ;
#1134 = CIRCLE('',#9198,0.025) ;
#1135 = CIRCLE('',#9200,0.025) ;
#1136 = CIRCLE('',#9201,0.025) ;
#1137 = CIRCLE('',#9203,0.025) ;
#1138 = CIRCLE('',#9317,0.025) ;
#1139 = CIRCLE('',#9321,0.35) ;
#1140 = CIRCLE('',#9322,0.2) ;
#1141 = CIRCLE('',#9324,0.35) ;
#1142 = CIRCLE('',#9325,0.2) ;
#1143 = CIRCLE('',#9328,0.2) ;
#1144 = CIRCLE('',#9330,0.2) ;
#1145 = CIRCLE('',#9340,0.21) ;
#1146 = CIRCLE('',#9341,0.21) ;
#1147 = CIRCLE('',#9351,0.025) ;
#1148 = CIRCLE('',#9352,0.025) ;
#1149 = CIRCLE('',#9354,0.025) ;
#1150 = CIRCLE('',#9355,0.025) ;
#1151 = CIRCLE('',#9356,0.025) ;
#1152 = CIRCLE('',#9358,0.025) ;
#1153 = CIRCLE('',#9359,0.025) ;
#1154 = CIRCLE('',#9360,0.025) ;
#1155 = CIRCLE('',#9361,0.025) ;
#1156 = CIRCLE('',#9363,0.025) ;
#1157 = CIRCLE('',#9364,0.025) ;
#1158 = CIRCLE('',#9365,0.025) ;
#1159 = CIRCLE('',#9366,0.025) ;
#1160 = CIRCLE('',#9368,0.025) ;
#1161 = CIRCLE('',#9369,0.025) ;
#1162 = CIRCLE('',#9370,0.025) ;
#1163 = CIRCLE('',#9371,0.025) ;
#1164 = CIRCLE('',#9373,0.025) ;
#1165 = CIRCLE('',#9374,0.025) ;
#1166 = CIRCLE('',#9375,0.025) ;
#1167 = CIRCLE('',#9377,0.025) ;
#1168 = CIRCLE('',#9378,0.025) ;
#1169 = CIRCLE('',#9380,0.025) ;
#1170 = CIRCLE('',#9381,0.025) ;
#1171 = CIRCLE('',#9383,0.025) ;
#1172 = CIRCLE('',#9384,0.025) ;
#1173 = CIRCLE('',#9386,0.025) ;
#1174 = CIRCLE('',#9387,0.025) ;
#1175 = CIRCLE('',#9388,0.025) ;
#1176 = CIRCLE('',#9390,0.025) ;
#1177 = CIRCLE('',#9391,0.025) ;
#1178 = CIRCLE('',#9392,0.025) ;
#1179 = CIRCLE('',#9393,0.025) ;
#1180 = CIRCLE('',#9395,0.025) ;
#1181 = CIRCLE('',#9396,0.025) ;
#1182 = CIRCLE('',#9397,0.025) ;
#1183 = CIRCLE('',#9398,0.025) ;
#1184 = CIRCLE('',#9400,0.025) ;
#1185 = CIRCLE('',#9401,0.025) ;
#1186 = CIRCLE('',#9402,0.025) ;
#1187 = CIRCLE('',#9403,0.025) ;
#1188 = CIRCLE('',#9405,0.025) ;
#1189 = CIRCLE('',#9406,0.025) ;
#1190 = CIRCLE('',#9407,0.025) ;
#1191 = CIRCLE('',#9409,0.025) ;
#1192 = CIRCLE('',#9410,0.025) ;
#1193 = CIRCLE('',#9412,0.025) ;
#1194 = CIRCLE('',#9413,0.025) ;
#1195 = CIRCLE('',#9415,0.025) ;
#1196 = CIRCLE('',#9416,0.025) ;
#1197 = CIRCLE('',#9418,0.025) ;
#1198 = CIRCLE('',#9419,0.025) ;
#1199 = CIRCLE('',#9420,0.025) ;
#1200 = CIRCLE('',#9422,0.025) ;
#1201 = CIRCLE('',#9423,0.025) ;
#1202 = CIRCLE('',#9424,0.025) ;
#1203 = CIRCLE('',#9425,0.025) ;
#1204 = CIRCLE('',#9427,0.025) ;
#1205 = CIRCLE('',#9428,0.025) ;
#1206 = CIRCLE('',#9429,0.025) ;
#1207 = CIRCLE('',#9430,0.025) ;
#1208 = CIRCLE('',#9432,0.025) ;
#1209 = CIRCLE('',#9433,0.025) ;
#1210 = CIRCLE('',#9434,0.025) ;
#1211 = CIRCLE('',#9435,0.025) ;
#1212 = CIRCLE('',#9437,0.025) ;
#1213 = CIRCLE('',#9438,0.025) ;
#1214 = CIRCLE('',#9439,0.025) ;
#1215 = CIRCLE('',#9441,0.025) ;
#1216 = CIRCLE('',#9442,0.025) ;
#1217 = CIRCLE('',#9444,0.025) ;
#1218 = CIRCLE('',#9512,0.025) ;
#1219 = CIRCLE('',#9516,0.15) ;
#1220 = CIRCLE('',#9517,0.15) ;
#1221 = CIRCLE('',#9527,0.15) ;
#1222 = CIRCLE('',#9528,0.15) ;
#1223 = CIRCLE('',#9532,0.15) ;
#1224 = CIRCLE('',#9533,0.15) ;
#1225 = CIRCLE('',#9538,0.15) ;
#1226 = CIRCLE('',#9539,0.15) ;
#1227 = CIRCLE('',#9544,0.15) ;
#1228 = CIRCLE('',#9545,0.15) ;
#1229 = CIRCLE('',#9550,0.02) ;
#1230 = CIRCLE('',#9551,0.02) ;
#1231 = CIRCLE('',#9553,0.02) ;
#1232 = CIRCLE('',#9554,0.02) ;
#1233 = CIRCLE('',#9555,0.02) ;
#1234 = CIRCLE('',#9557,0.02) ;
#1235 = CIRCLE('',#9558,0.02) ;
#1236 = CIRCLE('',#9559,0.02) ;
#1237 = CIRCLE('',#9560,0.02) ;
#1238 = CIRCLE('',#9562,0.02) ;
#1239 = CIRCLE('',#9563,0.02) ;
#1240 = CIRCLE('',#9564,0.02) ;
#1241 = CIRCLE('',#9565,0.02) ;
#1242 = CIRCLE('',#9567,0.02) ;
#1243 = CIRCLE('',#9568,0.02) ;
#1244 = CIRCLE('',#9569,0.02) ;
#1245 = CIRCLE('',#9570,0.02) ;
#1246 = CIRCLE('',#9572,0.02) ;
#1247 = CIRCLE('',#9573,0.02) ;
#1248 = CIRCLE('',#9574,0.02) ;
#1249 = CIRCLE('',#9576,0.02) ;
#1250 = CIRCLE('',#9577,0.02) ;
#1251 = CIRCLE('',#9579,0.02) ;
#1252 = CIRCLE('',#9580,0.02) ;
#1253 = CIRCLE('',#9582,0.02) ;
#1254 = CIRCLE('',#9583,0.02) ;
#1255 = CIRCLE('',#9585,0.02) ;
#1256 = CIRCLE('',#9586,0.02) ;
#1257 = CIRCLE('',#9587,0.02) ;
#1258 = CIRCLE('',#9589,0.02) ;
#1259 = CIRCLE('',#9590,0.02) ;
#1260 = CIRCLE('',#9591,0.02) ;
#1261 = CIRCLE('',#9592,0.02) ;
#1262 = CIRCLE('',#9594,0.02) ;
#1263 = CIRCLE('',#9595,0.02) ;
#1264 = CIRCLE('',#9596,0.02) ;
#1265 = CIRCLE('',#9597,0.02) ;
#1266 = CIRCLE('',#9599,0.02) ;
#1267 = CIRCLE('',#9600,0.02) ;
#1268 = CIRCLE('',#9601,0.02) ;
#1269 = CIRCLE('',#9602,0.02) ;
#1270 = CIRCLE('',#9604,0.02) ;
#1271 = CIRCLE('',#9605,0.02) ;
#1272 = CIRCLE('',#9606,0.02) ;
#1273 = CIRCLE('',#9608,0.02) ;
#1274 = CIRCLE('',#9609,0.02) ;
#1275 = CIRCLE('',#9611,0.02) ;
#1276 = CIRCLE('',#9612,0.02) ;
#1277 = CIRCLE('',#9614,0.02) ;
#1278 = CIRCLE('',#9615,0.02) ;
#1279 = CIRCLE('',#9617,0.02) ;
#1280 = CIRCLE('',#9618,0.02) ;
#1281 = CIRCLE('',#9619,0.02) ;
#1282 = CIRCLE('',#9621,0.02) ;
#1283 = CIRCLE('',#9622,0.02) ;
#1284 = CIRCLE('',#9623,0.02) ;
#1285 = CIRCLE('',#9624,0.02) ;
#1286 = CIRCLE('',#9626,0.02) ;
#1287 = CIRCLE('',#9627,0.02) ;
#1288 = CIRCLE('',#9628,0.02) ;
#1289 = CIRCLE('',#9629,0.02) ;
#1290 = CIRCLE('',#9631,0.02) ;
#1291 = CIRCLE('',#9632,0.02) ;
#1292 = CIRCLE('',#9633,0.02) ;
#1293 = CIRCLE('',#9634,0.02) ;
#1294 = CIRCLE('',#9636,0.02) ;
#1295 = CIRCLE('',#9637,0.02) ;
#1296 = CIRCLE('',#9638,0.02) ;
#1297 = CIRCLE('',#9640,0.02) ;
#1298 = CIRCLE('',#9641,0.02) ;
#1299 = CIRCLE('',#9643,0.02) ;
#1300 = CIRCLE('',#9644,0.02) ;
#1301 = CIRCLE('',#9646,0.02) ;
#1302 = CIRCLE('',#9647,0.02) ;
#1303 = CIRCLE('',#9649,0.02) ;
#1304 = CIRCLE('',#9650,0.02) ;
#1305 = CIRCLE('',#9651,0.02) ;
#1306 = CIRCLE('',#9653,0.02) ;
#1307 = CIRCLE('',#9654,0.02) ;
#1308 = CIRCLE('',#9655,0.02) ;
#1309 = CIRCLE('',#9656,0.02) ;
#1310 = CIRCLE('',#9658,0.02) ;
#1311 = CIRCLE('',#9659,0.02) ;
#1312 = CIRCLE('',#9660,0.02) ;
#1313 = CIRCLE('',#9661,0.02) ;
#1314 = CIRCLE('',#9663,0.02) ;
#1315 = CIRCLE('',#9664,0.02) ;
#1316 = CIRCLE('',#9665,0.02) ;
#1317 = CIRCLE('',#9666,0.02) ;
#1318 = CIRCLE('',#9668,0.02) ;
#1319 = CIRCLE('',#9669,0.02) ;
#1320 = CIRCLE('',#9670,0.02) ;
#1321 = CIRCLE('',#9672,0.02) ;
#1322 = CIRCLE('',#9673,0.02) ;
#1323 = CIRCLE('',#9675,0.02) ;
#1324 = CIRCLE('',#9766,0.02) ;
#1325 = CIRCLE('',#9782,0.08) ;
#1326 = CIRCLE('',#9783,0.08) ;
#1327 = CIRCLE('',#9800,0.16) ;
#1328 = CIRCLE('',#9802,0.16) ;
#1329 = CIRCLE('',#9811,0.15) ;
#1330 = CIRCLE('',#9812,0.15) ;
#1331 = CIRCLE('',#9814,0.15) ;
#1332 = CIRCLE('',#9816,0.15) ;
#1333 = CIRCLE('',#9819,0.025) ;
#1334 = CIRCLE('',#9820,0.025) ;
#1335 = CIRCLE('',#9824,0.025) ;
#1336 = CIRCLE('',#9825,0.025) ;
#1337 = CIRCLE('',#9830,0.115) ;
#1338 = CIRCLE('',#9831,0.115) ;
#1339 = CIRCLE('',#9835,0.025) ;
#1340 = CIRCLE('',#9836,0.025) ;
#1341 = CIRCLE('',#9840,0.025) ;
#1342 = CIRCLE('',#9841,0.025) ;
#1343 = CIRCLE('',#9846,0.21) ;
#1344 = CIRCLE('',#9847,0.21) ;
#1345 = CIRCLE('',#9851,0.21) ;
#1346 = CIRCLE('',#9852,0.21) ;
#1347 = CIRCLE('',#9857,0.21) ;
#1348 = CIRCLE('',#9858,0.21) ;
#1349 = CIRCLE('',#9865,0.2) ;
#1350 = CIRCLE('',#9866,0.2) ;
#1351 = CIRCLE('',#9870,0.04) ;
#1352 = CIRCLE('',#9871,0.04) ;
#1353 = CIRCLE('',#9875,0.04) ;
#1354 = CIRCLE('',#9876,0.04) ;
#1355 = CIRCLE('',#9881,0.29) ;
#1356 = CIRCLE('',#9882,0.29) ;
#1357 = CIRCLE('',#9897,0.15) ;
#1358 = CIRCLE('',#9898,0.15) ;
#1359 = CIRCLE('',#9901,0.275) ;
#1360 = CIRCLE('',#9902,0.275) ;
#1361 = CIRCLE('',#9907,0.15) ;
#1362 = CIRCLE('',#9908,0.15) ;
#1363 = CIRCLE('',#9911,0.275) ;
#1364 = CIRCLE('',#9912,0.275) ;
#1365 = FACE_OUTER_BOUND('',#1865,.T.) ;
#1366 = FACE_OUTER_BOUND('',#1866,.T.) ;
#1367 = FACE_OUTER_BOUND('',#1867,.T.) ;
#1368 = FACE_OUTER_BOUND('',#1868,.T.) ;
#1369 = FACE_OUTER_BOUND('',#1869,.T.) ;
#1370 = FACE_OUTER_BOUND('',#1870,.T.) ;
#1371 = FACE_OUTER_BOUND('',#1877,.T.) ;
#1372 = FACE_OUTER_BOUND('',#1878,.T.) ;
#1373 = FACE_OUTER_BOUND('',#1879,.T.) ;
#1374 = FACE_OUTER_BOUND('',#1880,.T.) ;
#1375 = FACE_OUTER_BOUND('',#1881,.T.) ;
#1376 = FACE_OUTER_BOUND('',#1882,.T.) ;
#1377 = FACE_OUTER_BOUND('',#1884,.T.) ;
#1378 = FACE_OUTER_BOUND('',#1885,.T.) ;
#1379 = FACE_OUTER_BOUND('',#1886,.T.) ;
#1380 = FACE_OUTER_BOUND('',#1887,.T.) ;
#1381 = FACE_OUTER_BOUND('',#1888,.T.) ;
#1382 = FACE_OUTER_BOUND('',#1889,.T.) ;
#1383 = FACE_OUTER_BOUND('',#1891,.T.) ;
#1384 = FACE_OUTER_BOUND('',#1892,.T.) ;
#1385 = FACE_OUTER_BOUND('',#1893,.T.) ;
#1386 = FACE_OUTER_BOUND('',#1894,.T.) ;
#1387 = FACE_OUTER_BOUND('',#1895,.T.) ;
#1388 = FACE_OUTER_BOUND('',#1896,.T.) ;
#1389 = FACE_OUTER_BOUND('',#1897,.T.) ;
#1390 = FACE_OUTER_BOUND('',#1899,.T.) ;
#1391 = FACE_OUTER_BOUND('',#1900,.T.) ;
#1392 = FACE_OUTER_BOUND('',#1901,.T.) ;
#1393 = FACE_OUTER_BOUND('',#1902,.T.) ;
#1394 = FACE_OUTER_BOUND('',#1904,.T.) ;
#1395 = FACE_OUTER_BOUND('',#1905,.T.) ;
#1396 = FACE_OUTER_BOUND('',#1906,.T.) ;
#1397 = FACE_OUTER_BOUND('',#1908,.T.) ;
#1398 = FACE_OUTER_BOUND('',#1909,.T.) ;
#1399 = FACE_OUTER_BOUND('',#1910,.T.) ;
#1400 = FACE_OUTER_BOUND('',#1911,.T.) ;
#1401 = FACE_OUTER_BOUND('',#1912,.T.) ;
#1402 = FACE_OUTER_BOUND('',#1914,.T.) ;
#1403 = FACE_OUTER_BOUND('',#1915,.T.) ;
#1404 = FACE_OUTER_BOUND('',#1917,.T.) ;
#1405 = FACE_OUTER_BOUND('',#1918,.T.) ;
#1406 = FACE_OUTER_BOUND('',#1919,.T.) ;
#1407 = FACE_OUTER_BOUND('',#1921,.T.) ;
#1408 = FACE_OUTER_BOUND('',#1922,.T.) ;
#1409 = FACE_OUTER_BOUND('',#1924,.T.) ;
#1410 = FACE_OUTER_BOUND('',#1925,.T.) ;
#1411 = FACE_OUTER_BOUND('',#1926,.T.) ;
#1412 = FACE_OUTER_BOUND('',#1927,.T.) ;
#1413 = FACE_OUTER_BOUND('',#1928,.T.) ;
#1414 = FACE_OUTER_BOUND('',#1929,.T.) ;
#1415 = FACE_OUTER_BOUND('',#1931,.T.) ;
#1416 = FACE_OUTER_BOUND('',#1937,.T.) ;
#1417 = FACE_OUTER_BOUND('',#1938,.T.) ;
#1418 = FACE_OUTER_BOUND('',#1939,.T.) ;
#1419 = FACE_OUTER_BOUND('',#1940,.T.) ;
#1420 = FACE_OUTER_BOUND('',#1942,.T.) ;
#1421 = FACE_OUTER_BOUND('',#1943,.T.) ;
#1422 = FACE_OUTER_BOUND('',#1945,.T.) ;
#1423 = FACE_OUTER_BOUND('',#1946,.T.) ;
#1424 = FACE_OUTER_BOUND('',#1947,.T.) ;
#1425 = FACE_OUTER_BOUND('',#1948,.T.) ;
#1426 = FACE_OUTER_BOUND('',#1949,.T.) ;
#1427 = FACE_OUTER_BOUND('',#1951,.T.) ;
#1428 = FACE_OUTER_BOUND('',#1952,.T.) ;
#1429 = FACE_OUTER_BOUND('',#1953,.T.) ;
#1430 = FACE_OUTER_BOUND('',#1954,.T.) ;
#1431 = FACE_OUTER_BOUND('',#1955,.T.) ;
#1432 = FACE_OUTER_BOUND('',#1956,.T.) ;
#1433 = FACE_OUTER_BOUND('',#1959,.T.) ;
#1434 = FACE_OUTER_BOUND('',#1960,.T.) ;
#1435 = FACE_OUTER_BOUND('',#1962,.T.) ;
#1436 = FACE_OUTER_BOUND('',#1963,.T.) ;
#1437 = FACE_OUTER_BOUND('',#1964,.T.) ;
#1438 = FACE_OUTER_BOUND('',#1965,.T.) ;
#1439 = FACE_OUTER_BOUND('',#1966,.T.) ;
#1440 = FACE_OUTER_BOUND('',#1967,.T.) ;
#1441 = FACE_OUTER_BOUND('',#1968,.T.) ;
#1442 = FACE_OUTER_BOUND('',#1969,.T.) ;
#1443 = FACE_OUTER_BOUND('',#1970,.T.) ;
#1444 = FACE_OUTER_BOUND('',#1971,.T.) ;
#1445 = FACE_OUTER_BOUND('',#1972,.T.) ;
#1446 = FACE_OUTER_BOUND('',#1973,.T.) ;
#1447 = FACE_OUTER_BOUND('',#1974,.T.) ;
#1448 = FACE_OUTER_BOUND('',#1975,.T.) ;
#1449 = FACE_OUTER_BOUND('',#1976,.T.) ;
#1450 = FACE_OUTER_BOUND('',#1977,.T.) ;
#1451 = FACE_OUTER_BOUND('',#1978,.T.) ;
#1452 = FACE_OUTER_BOUND('',#1979,.T.) ;
#1453 = FACE_OUTER_BOUND('',#1980,.T.) ;
#1454 = FACE_OUTER_BOUND('',#1981,.T.) ;
#1455 = FACE_OUTER_BOUND('',#1983,.T.) ;
#1456 = FACE_OUTER_BOUND('',#1985,.T.) ;
#1457 = FACE_OUTER_BOUND('',#1986,.T.) ;
#1458 = FACE_OUTER_BOUND('',#1987,.T.) ;
#1459 = FACE_OUTER_BOUND('',#1989,.T.) ;
#1460 = FACE_OUTER_BOUND('',#1991,.T.) ;
#1461 = FACE_OUTER_BOUND('',#1992,.T.) ;
#1462 = FACE_OUTER_BOUND('',#1994,.T.) ;
#1463 = FACE_OUTER_BOUND('',#1998,.T.) ;
#1464 = FACE_OUTER_BOUND('',#1999,.T.) ;
#1465 = FACE_OUTER_BOUND('',#2000,.T.) ;
#1466 = FACE_OUTER_BOUND('',#2002,.T.) ;
#1467 = FACE_OUTER_BOUND('',#2004,.T.) ;
#1468 = FACE_OUTER_BOUND('',#2005,.T.) ;
#1469 = FACE_OUTER_BOUND('',#2006,.T.) ;
#1470 = FACE_OUTER_BOUND('',#2008,.T.) ;
#1471 = FACE_OUTER_BOUND('',#2010,.T.) ;
#1472 = FACE_OUTER_BOUND('',#2011,.T.) ;
#1473 = FACE_OUTER_BOUND('',#2012,.T.) ;
#1474 = FACE_OUTER_BOUND('',#2013,.T.) ;
#1475 = FACE_OUTER_BOUND('',#2014,.T.) ;
#1476 = FACE_OUTER_BOUND('',#2015,.T.) ;
#1477 = FACE_OUTER_BOUND('',#2017,.T.) ;
#1478 = FACE_OUTER_BOUND('',#2018,.T.) ;
#1479 = FACE_OUTER_BOUND('',#2020,.T.) ;
#1480 = FACE_OUTER_BOUND('',#2022,.T.) ;
#1481 = FACE_OUTER_BOUND('',#2023,.T.) ;
#1482 = FACE_OUTER_BOUND('',#2024,.T.) ;
#1483 = FACE_OUTER_BOUND('',#2025,.T.) ;
#1484 = FACE_OUTER_BOUND('',#2026,.T.) ;
#1485 = FACE_OUTER_BOUND('',#2028,.T.) ;
#1486 = FACE_OUTER_BOUND('',#2029,.T.) ;
#1487 = FACE_OUTER_BOUND('',#2030,.T.) ;
#1488 = FACE_OUTER_BOUND('',#2031,.T.) ;
#1489 = FACE_OUTER_BOUND('',#2032,.T.) ;
#1490 = FACE_OUTER_BOUND('',#2033,.T.) ;
#1491 = FACE_OUTER_BOUND('',#2034,.T.) ;
#1492 = FACE_OUTER_BOUND('',#2035,.T.) ;
#1493 = FACE_OUTER_BOUND('',#2036,.T.) ;
#1494 = FACE_OUTER_BOUND('',#2037,.T.) ;
#1495 = FACE_OUTER_BOUND('',#2038,.T.) ;
#1496 = FACE_OUTER_BOUND('',#2039,.T.) ;
#1497 = FACE_OUTER_BOUND('',#2040,.T.) ;
#1498 = FACE_OUTER_BOUND('',#2041,.T.) ;
#1499 = FACE_OUTER_BOUND('',#2042,.T.) ;
#1500 = FACE_OUTER_BOUND('',#2044,.T.) ;
#1501 = FACE_OUTER_BOUND('',#2046,.T.) ;
#1502 = FACE_OUTER_BOUND('',#2049,.T.) ;
#1503 = FACE_OUTER_BOUND('',#2051,.T.) ;
#1504 = FACE_OUTER_BOUND('',#2053,.T.) ;
#1505 = FACE_OUTER_BOUND('',#2054,.T.) ;
#1506 = FACE_OUTER_BOUND('',#2055,.T.) ;
#1507 = FACE_OUTER_BOUND('',#2056,.T.) ;
#1508 = FACE_OUTER_BOUND('',#2057,.T.) ;
#1509 = FACE_OUTER_BOUND('',#2059,.T.) ;
#1510 = FACE_OUTER_BOUND('',#2060,.T.) ;
#1511 = FACE_OUTER_BOUND('',#2061,.T.) ;
#1512 = FACE_OUTER_BOUND('',#2063,.T.) ;
#1513 = FACE_OUTER_BOUND('',#2064,.T.) ;
#1514 = FACE_OUTER_BOUND('',#2065,.T.) ;
#1515 = FACE_OUTER_BOUND('',#2066,.T.) ;
#1516 = FACE_OUTER_BOUND('',#2067,.T.) ;
#1517 = FACE_OUTER_BOUND('',#2068,.T.) ;
#1518 = FACE_OUTER_BOUND('',#2069,.T.) ;
#1519 = FACE_OUTER_BOUND('',#2070,.T.) ;
#1520 = FACE_OUTER_BOUND('',#2071,.T.) ;
#1521 = FACE_OUTER_BOUND('',#2072,.T.) ;
#1522 = FACE_OUTER_BOUND('',#2074,.T.) ;
#1523 = FACE_OUTER_BOUND('',#2076,.T.) ;
#1524 = FACE_OUTER_BOUND('',#2077,.T.) ;
#1525 = FACE_OUTER_BOUND('',#2078,.T.) ;
#1526 = FACE_OUTER_BOUND('',#2080,.T.) ;
#1527 = FACE_OUTER_BOUND('',#2081,.T.) ;
#1528 = FACE_OUTER_BOUND('',#2083,.T.) ;
#1529 = FACE_OUTER_BOUND('',#2085,.T.) ;
#1530 = FACE_OUTER_BOUND('',#2086,.T.) ;
#1531 = FACE_OUTER_BOUND('',#2087,.T.) ;
#1532 = FACE_OUTER_BOUND('',#2088,.T.) ;
#1533 = FACE_OUTER_BOUND('',#2089,.T.) ;
#1534 = FACE_OUTER_BOUND('',#2090,.T.) ;
#1535 = FACE_OUTER_BOUND('',#2091,.T.) ;
#1536 = FACE_OUTER_BOUND('',#2092,.T.) ;
#1537 = FACE_OUTER_BOUND('',#2093,.T.) ;
#1538 = FACE_OUTER_BOUND('',#2094,.T.) ;
#1539 = FACE_OUTER_BOUND('',#2095,.T.) ;
#1540 = FACE_OUTER_BOUND('',#2097,.T.) ;
#1541 = FACE_OUTER_BOUND('',#2098,.T.) ;
#1542 = FACE_OUTER_BOUND('',#2099,.T.) ;
#1543 = FACE_OUTER_BOUND('',#2100,.T.) ;
#1544 = FACE_OUTER_BOUND('',#2101,.T.) ;
#1545 = FACE_OUTER_BOUND('',#2103,.T.) ;
#1546 = FACE_OUTER_BOUND('',#2104,.T.) ;
#1547 = FACE_OUTER_BOUND('',#2106,.T.) ;
#1548 = FACE_OUTER_BOUND('',#2108,.T.) ;
#1549 = FACE_OUTER_BOUND('',#2109,.T.) ;
#1550 = FACE_OUTER_BOUND('',#2111,.T.) ;
#1551 = FACE_OUTER_BOUND('',#2112,.T.) ;
#1552 = FACE_OUTER_BOUND('',#2113,.T.) ;
#1553 = FACE_OUTER_BOUND('',#2114,.T.) ;
#1554 = FACE_OUTER_BOUND('',#2115,.T.) ;
#1555 = FACE_OUTER_BOUND('',#2116,.T.) ;
#1556 = FACE_OUTER_BOUND('',#2117,.T.) ;
#1557 = FACE_OUTER_BOUND('',#2118,.T.) ;
#1558 = FACE_OUTER_BOUND('',#2119,.T.) ;
#1559 = FACE_OUTER_BOUND('',#2120,.T.) ;
#1560 = FACE_OUTER_BOUND('',#2121,.T.) ;
#1561 = FACE_OUTER_BOUND('',#2122,.T.) ;
#1562 = FACE_OUTER_BOUND('',#2123,.T.) ;
#1563 = FACE_OUTER_BOUND('',#2124,.T.) ;
#1564 = FACE_OUTER_BOUND('',#2125,.T.) ;
#1565 = FACE_OUTER_BOUND('',#2126,.T.) ;
#1566 = FACE_OUTER_BOUND('',#2127,.T.) ;
#1567 = FACE_OUTER_BOUND('',#2128,.T.) ;
#1568 = FACE_OUTER_BOUND('',#2129,.T.) ;
#1569 = FACE_OUTER_BOUND('',#2130,.T.) ;
#1570 = FACE_OUTER_BOUND('',#2131,.T.) ;
#1571 = FACE_OUTER_BOUND('',#2132,.T.) ;
#1572 = FACE_OUTER_BOUND('',#2133,.T.) ;
#1573 = FACE_OUTER_BOUND('',#2134,.T.) ;
#1574 = FACE_OUTER_BOUND('',#2135,.T.) ;
#1575 = FACE_OUTER_BOUND('',#2136,.T.) ;
#1576 = FACE_OUTER_BOUND('',#2137,.T.) ;
#1577 = FACE_OUTER_BOUND('',#2138,.T.) ;
#1578 = FACE_OUTER_BOUND('',#2139,.T.) ;
#1579 = FACE_OUTER_BOUND('',#2140,.T.) ;
#1580 = FACE_OUTER_BOUND('',#2141,.T.) ;
#1581 = FACE_OUTER_BOUND('',#2142,.T.) ;
#1582 = FACE_OUTER_BOUND('',#2143,.T.) ;
#1583 = FACE_OUTER_BOUND('',#2144,.T.) ;
#1584 = FACE_OUTER_BOUND('',#2145,.T.) ;
#1585 = FACE_OUTER_BOUND('',#2146,.T.) ;
#1586 = FACE_OUTER_BOUND('',#2147,.T.) ;
#1587 = FACE_OUTER_BOUND('',#2148,.T.) ;
#1588 = FACE_OUTER_BOUND('',#2149,.T.) ;
#1589 = FACE_OUTER_BOUND('',#2150,.T.) ;
#1590 = FACE_OUTER_BOUND('',#2151,.T.) ;
#1591 = FACE_OUTER_BOUND('',#2152,.T.) ;
#1592 = FACE_OUTER_BOUND('',#2153,.T.) ;
#1593 = FACE_OUTER_BOUND('',#2154,.T.) ;
#1594 = FACE_OUTER_BOUND('',#2155,.T.) ;
#1595 = FACE_OUTER_BOUND('',#2156,.T.) ;
#1596 = FACE_OUTER_BOUND('',#2157,.T.) ;
#1597 = FACE_OUTER_BOUND('',#2158,.T.) ;
#1598 = FACE_OUTER_BOUND('',#2159,.T.) ;
#1599 = FACE_OUTER_BOUND('',#2160,.T.) ;
#1600 = FACE_OUTER_BOUND('',#2161,.T.) ;
#1601 = FACE_OUTER_BOUND('',#2162,.T.) ;
#1602 = FACE_OUTER_BOUND('',#2163,.T.) ;
#1603 = FACE_OUTER_BOUND('',#2164,.T.) ;
#1604 = FACE_OUTER_BOUND('',#2165,.T.) ;
#1605 = FACE_OUTER_BOUND('',#2166,.T.) ;
#1606 = FACE_OUTER_BOUND('',#2167,.T.) ;
#1607 = FACE_OUTER_BOUND('',#2168,.T.) ;
#1608 = FACE_OUTER_BOUND('',#2169,.T.) ;
#1609 = FACE_OUTER_BOUND('',#2170,.T.) ;
#1610 = FACE_OUTER_BOUND('',#2171,.T.) ;
#1611 = FACE_OUTER_BOUND('',#2172,.T.) ;
#1612 = FACE_OUTER_BOUND('',#2173,.T.) ;
#1613 = FACE_OUTER_BOUND('',#2174,.T.) ;
#1614 = FACE_OUTER_BOUND('',#2175,.T.) ;
#1615 = FACE_OUTER_BOUND('',#2176,.T.) ;
#1616 = FACE_OUTER_BOUND('',#2177,.T.) ;
#1617 = FACE_OUTER_BOUND('',#2178,.T.) ;
#1618 = FACE_OUTER_BOUND('',#2179,.T.) ;
#1619 = FACE_OUTER_BOUND('',#2180,.T.) ;
#1620 = FACE_OUTER_BOUND('',#2181,.T.) ;
#1621 = FACE_OUTER_BOUND('',#2182,.T.) ;
#1622 = FACE_OUTER_BOUND('',#2183,.T.) ;
#1623 = FACE_OUTER_BOUND('',#2184,.T.) ;
#1624 = FACE_OUTER_BOUND('',#2185,.T.) ;
#1625 = FACE_OUTER_BOUND('',#2186,.T.) ;
#1626 = FACE_OUTER_BOUND('',#2187,.T.) ;
#1627 = FACE_OUTER_BOUND('',#2188,.T.) ;
#1628 = FACE_OUTER_BOUND('',#2189,.T.) ;
#1629 = FACE_OUTER_BOUND('',#2190,.T.) ;
#1630 = FACE_OUTER_BOUND('',#2191,.T.) ;
#1631 = FACE_OUTER_BOUND('',#2192,.T.) ;
#1632 = FACE_OUTER_BOUND('',#2193,.T.) ;
#1633 = FACE_OUTER_BOUND('',#2194,.T.) ;
#1634 = FACE_OUTER_BOUND('',#2195,.T.) ;
#1635 = FACE_OUTER_BOUND('',#2196,.T.) ;
#1636 = FACE_OUTER_BOUND('',#2198,.T.) ;
#1637 = FACE_OUTER_BOUND('',#2200,.T.) ;
#1638 = FACE_OUTER_BOUND('',#2201,.T.) ;
#1639 = FACE_OUTER_BOUND('',#2202,.T.) ;
#1640 = FACE_OUTER_BOUND('',#2203,.T.) ;
#1641 = FACE_OUTER_BOUND('',#2204,.T.) ;
#1642 = FACE_OUTER_BOUND('',#2205,.T.) ;
#1643 = FACE_OUTER_BOUND('',#2206,.T.) ;
#1644 = FACE_OUTER_BOUND('',#2207,.T.) ;
#1645 = FACE_OUTER_BOUND('',#2208,.T.) ;
#1646 = FACE_OUTER_BOUND('',#2209,.T.) ;
#1647 = FACE_OUTER_BOUND('',#2210,.T.) ;
#1648 = FACE_OUTER_BOUND('',#2211,.T.) ;
#1649 = FACE_OUTER_BOUND('',#2212,.T.) ;
#1650 = FACE_OUTER_BOUND('',#2214,.T.) ;
#1651 = FACE_OUTER_BOUND('',#2216,.T.) ;
#1652 = FACE_OUTER_BOUND('',#2217,.T.) ;
#1653 = FACE_OUTER_BOUND('',#2218,.T.) ;
#1654 = FACE_OUTER_BOUND('',#2219,.T.) ;
#1655 = FACE_OUTER_BOUND('',#2220,.T.) ;
#1656 = FACE_OUTER_BOUND('',#2221,.T.) ;
#1657 = FACE_OUTER_BOUND('',#2222,.T.) ;
#1658 = FACE_OUTER_BOUND('',#2223,.T.) ;
#1659 = FACE_OUTER_BOUND('',#2224,.T.) ;
#1660 = FACE_OUTER_BOUND('',#2225,.T.) ;
#1661 = FACE_OUTER_BOUND('',#2226,.T.) ;
#1662 = FACE_OUTER_BOUND('',#2227,.T.) ;
#1663 = FACE_OUTER_BOUND('',#2228,.T.) ;
#1664 = FACE_OUTER_BOUND('',#2229,.T.) ;
#1665 = FACE_OUTER_BOUND('',#2230,.T.) ;
#1666 = FACE_OUTER_BOUND('',#2231,.T.) ;
#1667 = FACE_OUTER_BOUND('',#2232,.T.) ;
#1668 = FACE_OUTER_BOUND('',#2233,.T.) ;
#1669 = FACE_OUTER_BOUND('',#2234,.T.) ;
#1670 = FACE_OUTER_BOUND('',#2235,.T.) ;
#1671 = FACE_OUTER_BOUND('',#2236,.T.) ;
#1672 = FACE_OUTER_BOUND('',#2237,.T.) ;
#1673 = FACE_OUTER_BOUND('',#2238,.T.) ;
#1674 = FACE_OUTER_BOUND('',#2239,.T.) ;
#1675 = FACE_OUTER_BOUND('',#2240,.T.) ;
#1676 = FACE_OUTER_BOUND('',#2241,.T.) ;
#1677 = FACE_OUTER_BOUND('',#2242,.T.) ;
#1678 = FACE_OUTER_BOUND('',#2243,.T.) ;
#1679 = FACE_OUTER_BOUND('',#2244,.T.) ;
#1680 = FACE_OUTER_BOUND('',#2245,.T.) ;
#1681 = FACE_OUTER_BOUND('',#2246,.T.) ;
#1682 = FACE_OUTER_BOUND('',#2247,.T.) ;
#1683 = FACE_OUTER_BOUND('',#2248,.T.) ;
#1684 = FACE_OUTER_BOUND('',#2249,.T.) ;
#1685 = FACE_OUTER_BOUND('',#2250,.T.) ;
#1686 = FACE_OUTER_BOUND('',#2251,.T.) ;
#1687 = FACE_OUTER_BOUND('',#2252,.T.) ;
#1688 = FACE_OUTER_BOUND('',#2253,.T.) ;
#1689 = FACE_OUTER_BOUND('',#2254,.T.) ;
#1690 = FACE_OUTER_BOUND('',#2255,.T.) ;
#1691 = FACE_OUTER_BOUND('',#2256,.T.) ;
#1692 = FACE_OUTER_BOUND('',#2257,.T.) ;
#1693 = FACE_OUTER_BOUND('',#2258,.T.) ;
#1694 = FACE_OUTER_BOUND('',#2259,.T.) ;
#1695 = FACE_OUTER_BOUND('',#2260,.T.) ;
#1696 = FACE_OUTER_BOUND('',#2261,.T.) ;
#1697 = FACE_OUTER_BOUND('',#2262,.T.) ;
#1698 = FACE_OUTER_BOUND('',#2263,.T.) ;
#1699 = FACE_OUTER_BOUND('',#2264,.T.) ;
#1700 = FACE_OUTER_BOUND('',#2265,.T.) ;
#1701 = FACE_OUTER_BOUND('',#2266,.T.) ;
#1702 = FACE_OUTER_BOUND('',#2267,.T.) ;
#1703 = FACE_OUTER_BOUND('',#2268,.T.) ;
#1704 = FACE_OUTER_BOUND('',#2269,.T.) ;
#1705 = FACE_OUTER_BOUND('',#2270,.T.) ;
#1706 = FACE_OUTER_BOUND('',#2271,.T.) ;
#1707 = FACE_OUTER_BOUND('',#2273,.T.) ;
#1708 = FACE_OUTER_BOUND('',#2274,.T.) ;
#1709 = FACE_OUTER_BOUND('',#2275,.T.) ;
#1710 = FACE_OUTER_BOUND('',#2276,.T.) ;
#1711 = FACE_OUTER_BOUND('',#2277,.T.) ;
#1712 = FACE_OUTER_BOUND('',#2278,.T.) ;
#1713 = FACE_OUTER_BOUND('',#2279,.T.) ;
#1714 = FACE_OUTER_BOUND('',#2280,.T.) ;
#1715 = FACE_OUTER_BOUND('',#2281,.T.) ;
#1716 = FACE_OUTER_BOUND('',#2282,.T.) ;
#1717 = FACE_OUTER_BOUND('',#2283,.T.) ;
#1718 = FACE_OUTER_BOUND('',#2284,.T.) ;
#1719 = FACE_OUTER_BOUND('',#2285,.T.) ;
#1720 = FACE_OUTER_BOUND('',#2286,.T.) ;
#1721 = FACE_OUTER_BOUND('',#2287,.T.) ;
#1722 = FACE_OUTER_BOUND('',#2288,.T.) ;
#1723 = FACE_OUTER_BOUND('',#2289,.T.) ;
#1724 = FACE_OUTER_BOUND('',#2290,.T.) ;
#1725 = FACE_OUTER_BOUND('',#2291,.T.) ;
#1726 = FACE_OUTER_BOUND('',#2292,.T.) ;
#1727 = FACE_OUTER_BOUND('',#2293,.T.) ;
#1728 = FACE_OUTER_BOUND('',#2294,.T.) ;
#1729 = FACE_OUTER_BOUND('',#2295,.T.) ;
#1730 = FACE_OUTER_BOUND('',#2296,.T.) ;
#1731 = FACE_OUTER_BOUND('',#2297,.T.) ;
#1732 = FACE_OUTER_BOUND('',#2298,.T.) ;
#1733 = FACE_OUTER_BOUND('',#2299,.T.) ;
#1734 = FACE_OUTER_BOUND('',#2300,.T.) ;
#1735 = FACE_OUTER_BOUND('',#2301,.T.) ;
#1736 = FACE_OUTER_BOUND('',#2302,.T.) ;
#1737 = FACE_OUTER_BOUND('',#2303,.T.) ;
#1738 = FACE_OUTER_BOUND('',#2304,.T.) ;
#1739 = FACE_OUTER_BOUND('',#2305,.T.) ;
#1740 = FACE_OUTER_BOUND('',#2306,.T.) ;
#1741 = FACE_OUTER_BOUND('',#2307,.T.) ;
#1742 = FACE_OUTER_BOUND('',#2308,.T.) ;
#1743 = FACE_OUTER_BOUND('',#2309,.T.) ;
#1744 = FACE_OUTER_BOUND('',#2310,.T.) ;
#1745 = FACE_OUTER_BOUND('',#2311,.T.) ;
#1746 = FACE_OUTER_BOUND('',#2312,.T.) ;
#1747 = FACE_OUTER_BOUND('',#2313,.T.) ;
#1748 = FACE_OUTER_BOUND('',#2314,.T.) ;
#1749 = FACE_OUTER_BOUND('',#2315,.T.) ;
#1750 = FACE_OUTER_BOUND('',#2316,.T.) ;
#1751 = FACE_OUTER_BOUND('',#2317,.T.) ;
#1752 = FACE_OUTER_BOUND('',#2318,.T.) ;
#1753 = FACE_OUTER_BOUND('',#2319,.T.) ;
#1754 = FACE_OUTER_BOUND('',#2320,.T.) ;
#1755 = FACE_OUTER_BOUND('',#2321,.T.) ;
#1756 = FACE_OUTER_BOUND('',#2322,.T.) ;
#1757 = FACE_OUTER_BOUND('',#2323,.T.) ;
#1758 = FACE_OUTER_BOUND('',#2324,.T.) ;
#1759 = FACE_OUTER_BOUND('',#2325,.T.) ;
#1760 = FACE_OUTER_BOUND('',#2326,.T.) ;
#1761 = FACE_OUTER_BOUND('',#2327,.T.) ;
#1762 = FACE_OUTER_BOUND('',#2328,.T.) ;
#1763 = FACE_OUTER_BOUND('',#2329,.T.) ;
#1764 = FACE_OUTER_BOUND('',#2330,.T.) ;
#1765 = FACE_OUTER_BOUND('',#2331,.T.) ;
#1766 = FACE_OUTER_BOUND('',#2332,.T.) ;
#1767 = FACE_OUTER_BOUND('',#2333,.T.) ;
#1768 = FACE_OUTER_BOUND('',#2334,.T.) ;
#1769 = FACE_OUTER_BOUND('',#2335,.T.) ;
#1770 = FACE_OUTER_BOUND('',#2336,.T.) ;
#1771 = FACE_OUTER_BOUND('',#2337,.T.) ;
#1772 = FACE_OUTER_BOUND('',#2338,.T.) ;
#1773 = FACE_OUTER_BOUND('',#2339,.T.) ;
#1774 = FACE_OUTER_BOUND('',#2340,.T.) ;
#1775 = FACE_OUTER_BOUND('',#2341,.T.) ;
#1776 = FACE_OUTER_BOUND('',#2342,.T.) ;
#1777 = FACE_OUTER_BOUND('',#2343,.T.) ;
#1778 = FACE_OUTER_BOUND('',#2344,.T.) ;
#1779 = FACE_OUTER_BOUND('',#2345,.T.) ;
#1780 = FACE_OUTER_BOUND('',#2346,.T.) ;
#1781 = FACE_OUTER_BOUND('',#2347,.T.) ;
#1782 = FACE_OUTER_BOUND('',#2348,.T.) ;
#1783 = FACE_OUTER_BOUND('',#2349,.T.) ;
#1784 = FACE_OUTER_BOUND('',#2350,.T.) ;
#1785 = FACE_OUTER_BOUND('',#2351,.T.) ;
#1786 = FACE_OUTER_BOUND('',#2352,.T.) ;
#1787 = FACE_OUTER_BOUND('',#2353,.T.) ;
#1788 = FACE_OUTER_BOUND('',#2354,.T.) ;
#1789 = FACE_OUTER_BOUND('',#2355,.T.) ;
#1790 = FACE_OUTER_BOUND('',#2356,.T.) ;
#1791 = FACE_OUTER_BOUND('',#2358,.T.) ;
#1792 = FACE_OUTER_BOUND('',#2359,.T.) ;
#1793 = FACE_OUTER_BOUND('',#2361,.T.) ;
#1794 = FACE_OUTER_BOUND('',#2362,.T.) ;
#1795 = FACE_OUTER_BOUND('',#2363,.T.) ;
#1796 = FACE_OUTER_BOUND('',#2364,.T.) ;
#1797 = FACE_OUTER_BOUND('',#2365,.T.) ;
#1798 = FACE_OUTER_BOUND('',#2366,.T.) ;
#1799 = FACE_OUTER_BOUND('',#2367,.T.) ;
#1800 = FACE_OUTER_BOUND('',#2368,.T.) ;
#1801 = FACE_OUTER_BOUND('',#2369,.T.) ;
#1802 = FACE_OUTER_BOUND('',#2370,.T.) ;
#1803 = FACE_OUTER_BOUND('',#2371,.T.) ;
#1804 = FACE_OUTER_BOUND('',#2372,.T.) ;
#1805 = FACE_OUTER_BOUND('',#2374,.T.) ;
#1806 = FACE_OUTER_BOUND('',#2375,.T.) ;
#1807 = FACE_OUTER_BOUND('',#2376,.T.) ;
#1808 = FACE_OUTER_BOUND('',#2377,.T.) ;
#1809 = FACE_OUTER_BOUND('',#2378,.T.) ;
#1810 = FACE_OUTER_BOUND('',#2380,.T.) ;
#1811 = FACE_OUTER_BOUND('',#2381,.T.) ;
#1812 = FACE_OUTER_BOUND('',#2383,.T.) ;
#1813 = FACE_OUTER_BOUND('',#2384,.T.) ;
#1814 = FACE_OUTER_BOUND('',#2385,.T.) ;
#1815 = FACE_OUTER_BOUND('',#2386,.T.) ;
#1816 = FACE_OUTER_BOUND('',#2387,.T.) ;
#1817 = FACE_OUTER_BOUND('',#2388,.T.) ;
#1818 = FACE_OUTER_BOUND('',#2389,.T.) ;
#1819 = FACE_OUTER_BOUND('',#2390,.T.) ;
#1820 = FACE_OUTER_BOUND('',#2391,.T.) ;
#1821 = FACE_OUTER_BOUND('',#2392,.T.) ;
#1822 = FACE_OUTER_BOUND('',#2393,.T.) ;
#1823 = FACE_OUTER_BOUND('',#2394,.T.) ;
#1824 = FACE_OUTER_BOUND('',#2395,.T.) ;
#1825 = FACE_OUTER_BOUND('',#2396,.T.) ;
#1826 = FACE_OUTER_BOUND('',#2397,.T.) ;
#1827 = FACE_OUTER_BOUND('',#2398,.T.) ;
#1828 = FACE_OUTER_BOUND('',#2399,.T.) ;
#1829 = FACE_OUTER_BOUND('',#2400,.T.) ;
#1830 = FACE_OUTER_BOUND('',#2401,.T.) ;
#1831 = FACE_OUTER_BOUND('',#2402,.T.) ;
#1832 = FACE_OUTER_BOUND('',#2403,.T.) ;
#1833 = FACE_OUTER_BOUND('',#2404,.T.) ;
#1834 = FACE_OUTER_BOUND('',#2405,.T.) ;
#1835 = FACE_OUTER_BOUND('',#2406,.T.) ;
#1836 = FACE_OUTER_BOUND('',#2407,.T.) ;
#1837 = FACE_OUTER_BOUND('',#2408,.T.) ;
#1838 = FACE_OUTER_BOUND('',#2409,.T.) ;
#1839 = FACE_OUTER_BOUND('',#2410,.T.) ;
#1840 = FACE_OUTER_BOUND('',#2411,.T.) ;
#1841 = FACE_OUTER_BOUND('',#2412,.T.) ;
#1842 = FACE_OUTER_BOUND('',#2414,.T.) ;
#1843 = FACE_OUTER_BOUND('',#2416,.T.) ;
#1844 = FACE_OUTER_BOUND('',#2417,.T.) ;
#1845 = FACE_OUTER_BOUND('',#2418,.T.) ;
#1846 = FACE_OUTER_BOUND('',#2419,.T.) ;
#1847 = FACE_OUTER_BOUND('',#2420,.T.) ;
#1848 = FACE_OUTER_BOUND('',#2421,.T.) ;
#1849 = FACE_OUTER_BOUND('',#2422,.T.) ;
#1850 = FACE_OUTER_BOUND('',#2423,.T.) ;
#1851 = FACE_OUTER_BOUND('',#2424,.T.) ;
#1852 = FACE_OUTER_BOUND('',#2425,.T.) ;
#1853 = FACE_OUTER_BOUND('',#2426,.T.) ;
#1854 = FACE_OUTER_BOUND('',#2427,.T.) ;
#1855 = FACE_OUTER_BOUND('',#2428,.T.) ;
#1856 = FACE_OUTER_BOUND('',#2429,.T.) ;
#1857 = FACE_OUTER_BOUND('',#2430,.T.) ;
#1858 = FACE_OUTER_BOUND('',#2431,.T.) ;
#1859 = FACE_OUTER_BOUND('',#2432,.T.) ;
#1860 = FACE_OUTER_BOUND('',#2434,.T.) ;
#1861 = FACE_OUTER_BOUND('',#2435,.T.) ;
#1862 = FACE_OUTER_BOUND('',#2436,.T.) ;
#1863 = FACE_OUTER_BOUND('',#2437,.T.) ;
#1864 = FACE_OUTER_BOUND('',#2438,.T.) ;
#1865 = EDGE_LOOP('',(#5273,#5274,#5275,#5276)) ;
#1866 = EDGE_LOOP('',(#5277,#5278,#5279,#5280,#5281,#5282)) ;
#1867 = EDGE_LOOP('',(#5283,#5284,#5285,#5286,#5287,#5288)) ;
#1868 = EDGE_LOOP('',(#5289,#5290,#5291,#5292)) ;
#1869 = EDGE_LOOP('',(#5293,#5294,#5295,#5296)) ;
#1870 = EDGE_LOOP('',(#5297,#5298,#5299,#5300,#5301,#5302)) ;
#1871 = EDGE_LOOP('',(#5303)) ;
#1872 = EDGE_LOOP('',(#5304)) ;
#1873 = EDGE_LOOP('',(#5305,#5306,#5307,#5308)) ;
#1874 = EDGE_LOOP('',(#5309,#5310,#5311,#5312)) ;
#1875 = EDGE_LOOP('',(#5313)) ;
#1876 = EDGE_LOOP('',(#5314)) ;
#1877 = EDGE_LOOP('',(#5315,#5316,#5317,#5318)) ;
#1878 = EDGE_LOOP('',(#5319)) ;
#1879 = EDGE_LOOP('',(#5320,#5321,#5322,#5323)) ;
#1880 = EDGE_LOOP('',(#5324)) ;
#1881 = EDGE_LOOP('',(#5325,#5326,#5327,#5328)) ;
#1882 = EDGE_LOOP('',(#5329,#5330,#5331,#5332)) ;
#1883 = EDGE_LOOP('',(#5333)) ;
#1884 = EDGE_LOOP('',(#5334,#5335,#5336,#5337)) ;
#1885 = EDGE_LOOP('',(#5338,#5339,#5340,#5341)) ;
#1886 = EDGE_LOOP('',(#5342,#5343,#5344,#5345)) ;
#1887 = EDGE_LOOP('',(#5346,#5347,#5348,#5349,#5350,#5351,#5352,#5353)) ;
#1888 = EDGE_LOOP('',(#5354,#5355,#5356,#5357)) ;
#1889 = EDGE_LOOP('',(#5358,#5359,#5360,#5361)) ;
#1890 = EDGE_LOOP('',(#5362)) ;
#1891 = EDGE_LOOP('',(#5363,#5364,#5365,#5366)) ;
#1892 = EDGE_LOOP('',(#5367,#5368,#5369,#5370)) ;
#1893 = EDGE_LOOP('',(#5371,#5372,#5373,#5374)) ;
#1894 = EDGE_LOOP('',(#5375,#5376,#5377,#5378,#5379,#5380,#5381,#5382)) ;
#1895 = EDGE_LOOP('',(#5383,#5384,#5385,#5386)) ;
#1896 = EDGE_LOOP('',(#5387,#5388,#5389,#5390)) ;
#1897 = EDGE_LOOP('',(#5391)) ;
#1898 = EDGE_LOOP('',(#5392)) ;
#1899 = EDGE_LOOP('',(#5393)) ;
#1900 = EDGE_LOOP('',(#5394,#5395,#5396,#5397)) ;
#1901 = EDGE_LOOP('',(#5398,#5399,#5400,#5401)) ;
#1902 = EDGE_LOOP('',(#5402)) ;
#1903 = EDGE_LOOP('',(#5403)) ;
#1904 = EDGE_LOOP('',(#5404,#5405,#5406,#5407)) ;
#1905 = EDGE_LOOP('',(#5408,#5409,#5410,#5411)) ;
#1906 = EDGE_LOOP('',(#5412)) ;
#1907 = EDGE_LOOP('',(#5413)) ;
#1908 = EDGE_LOOP('',(#5414)) ;
#1909 = EDGE_LOOP('',(#5415,#5416,#5417,#5418)) ;
#1910 = EDGE_LOOP('',(#5419,#5420,#5421,#5422)) ;
#1911 = EDGE_LOOP('',(#5423,#5424,#5425,#5426)) ;
#1912 = EDGE_LOOP('',(#5427,#5428,#5429,#5430)) ;
#1913 = EDGE_LOOP('',(#5431)) ;
#1914 = EDGE_LOOP('',(#5432,#5433,#5434,#5435)) ;
#1915 = EDGE_LOOP('',(#5436,#5437,#5438,#5439)) ;
#1916 = EDGE_LOOP('',(#5440)) ;
#1917 = EDGE_LOOP('',(#5441,#5442,#5443,#5444)) ;
#1918 = EDGE_LOOP('',(#5445,#5446,#5447,#5448)) ;
#1919 = EDGE_LOOP('',(#5449,#5450,#5451,#5452)) ;
#1920 = EDGE_LOOP('',(#5453)) ;
#1921 = EDGE_LOOP('',(#5454,#5455,#5456,#5457)) ;
#1922 = EDGE_LOOP('',(#5458,#5459,#5460,#5461)) ;
#1923 = EDGE_LOOP('',(#5462)) ;
#1924 = EDGE_LOOP('',(#5463,#5464,#5465,#5466)) ;
#1925 = EDGE_LOOP('',(#5467,#5468,#5469,#5470)) ;
#1926 = EDGE_LOOP('',(#5471,#5472,#5473,#5474)) ;
#1927 = EDGE_LOOP('',(#5475,#5476,#5477,#5478)) ;
#1928 = EDGE_LOOP('',(#5479)) ;
#1929 = EDGE_LOOP('',(#5480,#5481,#5482,#5483)) ;
#1930 = EDGE_LOOP('',(#5484,#5485,#5486,#5487)) ;
#1931 = EDGE_LOOP('',(#5488,#5489,#5490,#5491,#5492,#5493,#5494,#5495,#5496,
#5497,#5498,#5499)) ;
#1932 = EDGE_LOOP('',(#5500)) ;
#1933 = EDGE_LOOP('',(#5501)) ;
#1934 = EDGE_LOOP('',(#5502)) ;
#1935 = EDGE_LOOP('',(#5503)) ;
#1936 = EDGE_LOOP('',(#5504)) ;
#1937 = EDGE_LOOP('',(#5505,#5506,#5507,#5508)) ;
#1938 = EDGE_LOOP('',(#5509,#5510,#5511,#5512)) ;
#1939 = EDGE_LOOP('',(#5513,#5514,#5515,#5516)) ;
#1940 = EDGE_LOOP('',(#5517,#5518,#5519,#5520)) ;
#1941 = EDGE_LOOP('',(#5521)) ;
#1942 = EDGE_LOOP('',(#5522,#5523,#5524,#5525)) ;
#1943 = EDGE_LOOP('',(#5526,#5527,#5528,#5529,#5530,#5531,#5532,#5533)) ;
#1944 = EDGE_LOOP('',(#5534)) ;
#1945 = EDGE_LOOP('',(#5535,#5536,#5537)) ;
#1946 = EDGE_LOOP('',(#5538,#5539,#5540,#5541)) ;
#1947 = EDGE_LOOP('',(#5542,#5543,#5544,#5545)) ;
#1948 = EDGE_LOOP('',(#5546,#5547,#5548,#5549)) ;
#1949 = EDGE_LOOP('',(#5550,#5551,#5552,#5553)) ;
#1950 = EDGE_LOOP('',(#5554)) ;
#1951 = EDGE_LOOP('',(#5555,#5556,#5557,#5558,#5559,#5560,#5561,#5562,#5563,
#5564,#5565,#5566)) ;
#1952 = EDGE_LOOP('',(#5567,#5568,#5569)) ;
#1953 = EDGE_LOOP('',(#5570,#5571,#5572,#5573,#5574,#5575)) ;
#1954 = EDGE_LOOP('',(#5576,#5577,#5578,#5579)) ;
#1955 = EDGE_LOOP('',(#5580,#5581,#5582,#5583)) ;
#1956 = EDGE_LOOP('',(#5584,#5585,#5586,#5587)) ;
#1957 = EDGE_LOOP('',(#5588)) ;
#1958 = EDGE_LOOP('',(#5589)) ;
#1959 = EDGE_LOOP('',(#5590,#5591,#5592,#5593)) ;
#1960 = EDGE_LOOP('',(#5594,#5595,#5596,#5597,#5598,#5599,#5600,#5601)) ;
#1961 = EDGE_LOOP('',(#5602)) ;
#1962 = EDGE_LOOP('',(#5603,#5604,#5605,#5606)) ;
#1963 = EDGE_LOOP('',(#5607)) ;
#1964 = EDGE_LOOP('',(#5608,#5609,#5610,#5611)) ;
#1965 = EDGE_LOOP('',(#5612,#5613,#5614,#5615)) ;
#1966 = EDGE_LOOP('',(#5616,#5617,#5618,#5619)) ;
#1967 = EDGE_LOOP('',(#5620,#5621,#5622,#5623)) ;
#1968 = EDGE_LOOP('',(#5624,#5625,#5626,#5627)) ;
#1969 = EDGE_LOOP('',(#5628,#5629,#5630,#5631)) ;
#1970 = EDGE_LOOP('',(#5632,#5633,#5634,#5635)) ;
#1971 = EDGE_LOOP('',(#5636,#5637,#5638,#5639)) ;
#1972 = EDGE_LOOP('',(#5640,#5641,#5642,#5643)) ;
#1973 = EDGE_LOOP('',(#5644,#5645,#5646,#5647)) ;
#1974 = EDGE_LOOP('',(#5648,#5649,#5650,#5651)) ;
#1975 = EDGE_LOOP('',(#5652,#5653,#5654,#5655)) ;
#1976 = EDGE_LOOP('',(#5656,#5657,#5658,#5659)) ;
#1977 = EDGE_LOOP('',(#5660,#5661,#5662,#5663)) ;
#1978 = EDGE_LOOP('',(#5664,#5665,#5666,#5667)) ;
#1979 = EDGE_LOOP('',(#5668,#5669,#5670,#5671)) ;
#1980 = EDGE_LOOP('',(#5672,#5673,#5674,#5675)) ;
#1981 = EDGE_LOOP('',(#5676)) ;
#1982 = EDGE_LOOP('',(#5677)) ;
#1983 = EDGE_LOOP('',(#5678)) ;
#1984 = EDGE_LOOP('',(#5679)) ;
#1985 = EDGE_LOOP('',(#5680,#5681,#5682,#5683)) ;
#1986 = EDGE_LOOP('',(#5684,#5685,#5686,#5687)) ;
#1987 = EDGE_LOOP('',(#5688)) ;
#1988 = EDGE_LOOP('',(#5689)) ;
#1989 = EDGE_LOOP('',(#5690)) ;
#1990 = EDGE_LOOP('',(#5691)) ;
#1991 = EDGE_LOOP('',(#5692,#5693,#5694,#5695)) ;
#1992 = EDGE_LOOP('',(#5696)) ;
#1993 = EDGE_LOOP('',(#5697)) ;
#1994 = EDGE_LOOP('',(#5698)) ;
#1995 = EDGE_LOOP('',(#5699,#5700,#5701,#5702)) ;
#1996 = EDGE_LOOP('',(#5703,#5704,#5705,#5706)) ;
#1997 = EDGE_LOOP('',(#5707,#5708,#5709,#5710)) ;
#1998 = EDGE_LOOP('',(#5711,#5712,#5713,#5714)) ;
#1999 = EDGE_LOOP('',(#5715,#5716,#5717,#5718)) ;
#2000 = EDGE_LOOP('',(#5719)) ;
#2001 = EDGE_LOOP('',(#5720)) ;
#2002 = EDGE_LOOP('',(#5721)) ;
#2003 = EDGE_LOOP('',(#5722)) ;
#2004 = EDGE_LOOP('',(#5723,#5724,#5725,#5726)) ;
#2005 = EDGE_LOOP('',(#5727,#5728,#5729,#5730)) ;
#2006 = EDGE_LOOP('',(#5731)) ;
#2007 = EDGE_LOOP('',(#5732)) ;
#2008 = EDGE_LOOP('',(#5733)) ;
#2009 = EDGE_LOOP('',(#5734)) ;
#2010 = EDGE_LOOP('',(#5735,#5736,#5737)) ;
#2011 = EDGE_LOOP('',(#5738,#5739,#5740,#5741)) ;
#2012 = EDGE_LOOP('',(#5742)) ;
#2013 = EDGE_LOOP('',(#5743,#5744,#5745,#5746)) ;
#2014 = EDGE_LOOP('',(#5747,#5748,#5749,#5750)) ;
#2015 = EDGE_LOOP('',(#5751)) ;
#2016 = EDGE_LOOP('',(#5752)) ;
#2017 = EDGE_LOOP('',(#5753,#5754,#5755,#5756)) ;
#2018 = EDGE_LOOP('',(#5757)) ;
#2019 = EDGE_LOOP('',(#5758)) ;
#2020 = EDGE_LOOP('',(#5759)) ;
#2021 = EDGE_LOOP('',(#5760)) ;
#2022 = EDGE_LOOP('',(#5761,#5762,#5763,#5764)) ;
#2023 = EDGE_LOOP('',(#5765)) ;
#2024 = EDGE_LOOP('',(#5766,#5767,#5768,#5769)) ;
#2025 = EDGE_LOOP('',(#5770)) ;
#2026 = EDGE_LOOP('',(#5771)) ;
#2027 = EDGE_LOOP('',(#5772)) ;
#2028 = EDGE_LOOP('',(#5773,#5774,#5775,#5776)) ;
#2029 = EDGE_LOOP('',(#5777)) ;
#2030 = EDGE_LOOP('',(#5778)) ;
#2031 = EDGE_LOOP('',(#5779,#5780,#5781,#5782)) ;
#2032 = EDGE_LOOP('',(#5783,#5784,#5785)) ;
#2033 = EDGE_LOOP('',(#5786,#5787,#5788,#5789)) ;
#2034 = EDGE_LOOP('',(#5790,#5791,#5792)) ;
#2035 = EDGE_LOOP('',(#5793,#5794,#5795)) ;
#2036 = EDGE_LOOP('',(#5796,#5797,#5798)) ;
#2037 = EDGE_LOOP('',(#5799,#5800,#5801,#5802)) ;
#2038 = EDGE_LOOP('',(#5803,#5804,#5805,#5806)) ;
#2039 = EDGE_LOOP('',(#5807,#5808,#5809,#5810)) ;
#2040 = EDGE_LOOP('',(#5811,#5812)) ;
#2041 = EDGE_LOOP('',(#5813,#5814,#5815,#5816,#5817,#5818,#5819,#5820)) ;
#2042 = EDGE_LOOP('',(#5821,#5822,#5823,#5824,#5825,#5826,#5827,#5828)) ;
#2043 = EDGE_LOOP('',(#5829,#5830,#5831,#5832)) ;
#2044 = EDGE_LOOP('',(#5833,#5834,#5835,#5836)) ;
#2045 = EDGE_LOOP('',(#5837)) ;
#2046 = EDGE_LOOP('',(#5838)) ;
#2047 = EDGE_LOOP('',(#5839)) ;
#2048 = EDGE_LOOP('',(#5840)) ;
#2049 = EDGE_LOOP('',(#5841,#5842,#5843,#5844)) ;
#2050 = EDGE_LOOP('',(#5845,#5846,#5847,#5848)) ;
#2051 = EDGE_LOOP('',(#5849)) ;
#2052 = EDGE_LOOP('',(#5850)) ;
#2053 = EDGE_LOOP('',(#5851,#5852)) ;
#2054 = EDGE_LOOP('',(#5853,#5854)) ;
#2055 = EDGE_LOOP('',(#5855,#5856)) ;
#2056 = EDGE_LOOP('',(#5857,#5858)) ;
#2057 = EDGE_LOOP('',(#5859)) ;
#2058 = EDGE_LOOP('',(#5860)) ;
#2059 = EDGE_LOOP('',(#5861,#5862)) ;
#2060 = EDGE_LOOP('',(#5863,#5864,#5865,#5866,#5867,#5868)) ;
#2061 = EDGE_LOOP('',(#5869)) ;
#2062 = EDGE_LOOP('',(#5870)) ;
#2063 = EDGE_LOOP('',(#5871,#5872)) ;
#2064 = EDGE_LOOP('',(#5873,#5874,#5875,#5876,#5877,#5878)) ;
#2065 = EDGE_LOOP('',(#5879,#5880,#5881,#5882,#5883,#5884)) ;
#2066 = EDGE_LOOP('',(#5885,#5886,#5887,#5888,#5889,#5890)) ;
#2067 = EDGE_LOOP('',(#5891,#5892,#5893,#5894)) ;
#2068 = EDGE_LOOP('',(#5895,#5896,#5897)) ;
#2069 = EDGE_LOOP('',(#5898,#5899,#5900)) ;
#2070 = EDGE_LOOP('',(#5901,#5902,#5903,#5904)) ;
#2071 = EDGE_LOOP('',(#5905,#5906,#5907,#5908)) ;
#2072 = EDGE_LOOP('',(#5909)) ;
#2073 = EDGE_LOOP('',(#5910)) ;
#2074 = EDGE_LOOP('',(#5911)) ;
#2075 = EDGE_LOOP('',(#5912)) ;
#2076 = EDGE_LOOP('',(#5913,#5914,#5915,#5916)) ;
#2077 = EDGE_LOOP('',(#5917,#5918,#5919,#5920)) ;
#2078 = EDGE_LOOP('',(#5921)) ;
#2079 = EDGE_LOOP('',(#5922)) ;
#2080 = EDGE_LOOP('',(#5923,#5924,#5925,#5926)) ;
#2081 = EDGE_LOOP('',(#5927)) ;
#2082 = EDGE_LOOP('',(#5928)) ;
#2083 = EDGE_LOOP('',(#5929)) ;
#2084 = EDGE_LOOP('',(#5930)) ;
#2085 = EDGE_LOOP('',(#5931,#5932,#5933,#5934)) ;
#2086 = EDGE_LOOP('',(#5935)) ;
#2087 = EDGE_LOOP('',(#5936)) ;
#2088 = EDGE_LOOP('',(#5937,#5938,#5939,#5940)) ;
#2089 = EDGE_LOOP('',(#5941)) ;
#2090 = EDGE_LOOP('',(#5942)) ;
#2091 = EDGE_LOOP('',(#5943,#5944,#5945,#5946)) ;
#2092 = EDGE_LOOP('',(#5947,#5948,#5949,#5950)) ;
#2093 = EDGE_LOOP('',(#5951,#5952,#5953,#5954)) ;
#2094 = EDGE_LOOP('',(#5955,#5956,#5957,#5958)) ;
#2095 = EDGE_LOOP('',(#5959,#5960,#5961,#5962,#5963,#5964,#5965,#5966,#5967,
#5968)) ;
#2096 = EDGE_LOOP('',(#5969)) ;
#2097 = EDGE_LOOP('',(#5970,#5971,#5972,#5973)) ;
#2098 = EDGE_LOOP('',(#5974,#5975,#5976,#5977)) ;
#2099 = EDGE_LOOP('',(#5978,#5979,#5980,#5981)) ;
#2100 = EDGE_LOOP('',(#5982,#5983,#5984,#5985)) ;
#2101 = EDGE_LOOP('',(#5986,#5987,#5988,#5989)) ;
#2102 = EDGE_LOOP('',(#5990)) ;
#2103 = EDGE_LOOP('',(#5991,#5992,#5993,#5994)) ;
#2104 = EDGE_LOOP('',(#5995,#5996,#5997,#5998,#5999,#6000,#6001,#6002,#6003,
#6004)) ;
#2105 = EDGE_LOOP('',(#6005)) ;
#2106 = EDGE_LOOP('',(#6006,#6007,#6008,#6009)) ;
#2107 = EDGE_LOOP('',(#6010)) ;
#2108 = EDGE_LOOP('',(#6011,#6012,#6013,#6014)) ;
#2109 = EDGE_LOOP('',(#6015)) ;
#2110 = EDGE_LOOP('',(#6016)) ;
#2111 = EDGE_LOOP('',(#6017,#6018,#6019,#6020)) ;
#2112 = EDGE_LOOP('',(#6021)) ;
#2113 = EDGE_LOOP('',(#6022,#6023,#6024,#6025)) ;
#2114 = EDGE_LOOP('',(#6026)) ;
#2115 = EDGE_LOOP('',(#6027,#6028)) ;
#2116 = EDGE_LOOP('',(#6029,#6030,#6031)) ;
#2117 = EDGE_LOOP('',(#6032,#6033,#6034,#6035)) ;
#2118 = EDGE_LOOP('',(#6036,#6037,#6038,#6039)) ;
#2119 = EDGE_LOOP('',(#6040,#6041,#6042,#6043)) ;
#2120 = EDGE_LOOP('',(#6044,#6045,#6046)) ;
#2121 = EDGE_LOOP('',(#6047,#6048)) ;
#2122 = EDGE_LOOP('',(#6049,#6050)) ;
#2123 = EDGE_LOOP('',(#6051,#6052)) ;
#2124 = EDGE_LOOP('',(#6053,#6054,#6055)) ;
#2125 = EDGE_LOOP('',(#6056,#6057,#6058,#6059)) ;
#2126 = EDGE_LOOP('',(#6060,#6061,#6062,#6063)) ;
#2127 = EDGE_LOOP('',(#6064,#6065,#6066,#6067)) ;
#2128 = EDGE_LOOP('',(#6068,#6069,#6070)) ;
#2129 = EDGE_LOOP('',(#6071,#6072)) ;
#2130 = EDGE_LOOP('',(#6073,#6074)) ;
#2131 = EDGE_LOOP('',(#6075,#6076)) ;
#2132 = EDGE_LOOP('',(#6077,#6078,#6079)) ;
#2133 = EDGE_LOOP('',(#6080,#6081,#6082,#6083)) ;
#2134 = EDGE_LOOP('',(#6084,#6085,#6086,#6087)) ;
#2135 = EDGE_LOOP('',(#6088,#6089,#6090,#6091)) ;
#2136 = EDGE_LOOP('',(#6092,#6093,#6094)) ;
#2137 = EDGE_LOOP('',(#6095,#6096)) ;
#2138 = EDGE_LOOP('',(#6097,#6098)) ;
#2139 = EDGE_LOOP('',(#6099,#6100)) ;
#2140 = EDGE_LOOP('',(#6101,#6102,#6103)) ;
#2141 = EDGE_LOOP('',(#6104,#6105,#6106,#6107)) ;
#2142 = EDGE_LOOP('',(#6108,#6109,#6110,#6111)) ;
#2143 = EDGE_LOOP('',(#6112,#6113,#6114,#6115)) ;
#2144 = EDGE_LOOP('',(#6116,#6117,#6118)) ;
#2145 = EDGE_LOOP('',(#6119,#6120)) ;
#2146 = EDGE_LOOP('',(#6121,#6122)) ;
#2147 = EDGE_LOOP('',(#6123,#6124)) ;
#2148 = EDGE_LOOP('',(#6125,#6126,#6127)) ;
#2149 = EDGE_LOOP('',(#6128,#6129,#6130,#6131)) ;
#2150 = EDGE_LOOP('',(#6132,#6133,#6134,#6135)) ;
#2151 = EDGE_LOOP('',(#6136,#6137,#6138,#6139)) ;
#2152 = EDGE_LOOP('',(#6140,#6141,#6142)) ;
#2153 = EDGE_LOOP('',(#6143,#6144)) ;
#2154 = EDGE_LOOP('',(#6145,#6146,#6147,#6148,#6149,#6150,#6151)) ;
#2155 = EDGE_LOOP('',(#6152)) ;
#2156 = EDGE_LOOP('',(#6153,#6154,#6155,#6156,#6157,#6158,#6159,#6160,#6161)) ;
#2157 = EDGE_LOOP('',(#6162,#6163,#6164,#6165,#6166,#6167,#6168,#6169,#6170)) ;
#2158 = EDGE_LOOP('',(#6171,#6172,#6173,#6174,#6175,#6176,#6177,#6178)) ;
#2159 = EDGE_LOOP('',(#6179,#6180,#6181,#6182,#6183,#6184,#6185,#6186)) ;
#2160 = EDGE_LOOP('',(#6187,#6188,#6189,#6190,#6191,#6192,#6193,#6194,#6195)) ;
#2161 = EDGE_LOOP('',(#6196,#6197,#6198,#6199,#6200,#6201,#6202,#6203,#6204)) ;
#2162 = EDGE_LOOP('',(#6205,#6206,#6207,#6208,#6209,#6210,#6211,#6212,#6213)) ;
#2163 = EDGE_LOOP('',(#6214,#6215,#6216,#6217,#6218,#6219,#6220,#6221,#6222)) ;
#2164 = EDGE_LOOP('',(#6223,#6224,#6225,#6226,#6227,#6228,#6229,#6230,#6231)) ;
#2165 = EDGE_LOOP('',(#6232,#6233,#6234,#6235,#6236,#6237,#6238,#6239,#6240)) ;
#2166 = EDGE_LOOP('',(#6241,#6242,#6243,#6244,#6245,#6246,#6247,#6248)) ;
#2167 = EDGE_LOOP('',(#6249,#6250,#6251,#6252,#6253,#6254,#6255,#6256)) ;
#2168 = EDGE_LOOP('',(#6257,#6258,#6259,#6260,#6261,#6262,#6263,#6264,#6265)) ;
#2169 = EDGE_LOOP('',(#6266,#6267,#6268,#6269,#6270,#6271,#6272,#6273,#6274)) ;
#2170 = EDGE_LOOP('',(#6275,#6276,#6277,#6278,#6279,#6280,#6281,#6282,#6283)) ;
#2171 = EDGE_LOOP('',(#6284,#6285,#6286,#6287,#6288,#6289,#6290,#6291,#6292)) ;
#2172 = EDGE_LOOP('',(#6293,#6294,#6295,#6296,#6297,#6298,#6299,#6300,#6301)) ;
#2173 = EDGE_LOOP('',(#6302,#6303,#6304,#6305,#6306,#6307,#6308,#6309,#6310)) ;
#2174 = EDGE_LOOP('',(#6311,#6312,#6313,#6314,#6315,#6316,#6317,#6318)) ;
#2175 = EDGE_LOOP('',(#6319,#6320,#6321,#6322,#6323,#6324,#6325,#6326)) ;
#2176 = EDGE_LOOP('',(#6327,#6328,#6329,#6330,#6331,#6332,#6333,#6334,#6335)) ;
#2177 = EDGE_LOOP('',(#6336,#6337,#6338,#6339,#6340,#6341,#6342,#6343,#6344)) ;
#2178 = EDGE_LOOP('',(#6345,#6346,#6347,#6348,#6349,#6350,#6351,#6352,#6353)) ;
#2179 = EDGE_LOOP('',(#6354,#6355,#6356,#6357,#6358,#6359,#6360,#6361,#6362)) ;
#2180 = EDGE_LOOP('',(#6363,#6364,#6365,#6366,#6367,#6368,#6369,#6370,#6371)) ;
#2181 = EDGE_LOOP('',(#6372,#6373,#6374,#6375,#6376,#6377,#6378,#6379,#6380)) ;
#2182 = EDGE_LOOP('',(#6381,#6382,#6383,#6384,#6385,#6386,#6387,#6388)) ;
#2183 = EDGE_LOOP('',(#6389,#6390,#6391,#6392,#6393,#6394,#6395,#6396)) ;
#2184 = EDGE_LOOP('',(#6397,#6398,#6399,#6400,#6401,#6402,#6403,#6404,#6405)) ;
#2185 = EDGE_LOOP('',(#6406,#6407,#6408,#6409,#6410,#6411,#6412,#6413,#6414)) ;
#2186 = EDGE_LOOP('',(#6415,#6416,#6417,#6418,#6419,#6420,#6421,#6422,#6423)) ;
#2187 = EDGE_LOOP('',(#6424,#6425,#6426,#6427,#6428,#6429,#6430,#6431,#6432)) ;
#2188 = EDGE_LOOP('',(#6433,#6434,#6435,#6436,#6437,#6438,#6439,#6440,#6441)) ;
#2189 = EDGE_LOOP('',(#6442,#6443,#6444,#6445,#6446,#6447,#6448,#6449,#6450)) ;
#2190 = EDGE_LOOP('',(#6451,#6452,#6453,#6454,#6455,#6456,#6457,#6458)) ;
#2191 = EDGE_LOOP('',(#6459,#6460,#6461,#6462,#6463,#6464,#6465,#6466)) ;
#2192 = EDGE_LOOP('',(#6467,#6468,#6469,#6470,#6471,#6472,#6473,#6474,#6475)) ;
#2193 = EDGE_LOOP('',(#6476,#6477,#6478,#6479,#6480,#6481,#6482,#6483,#6484)) ;
#2194 = EDGE_LOOP('',(#6485,#6486,#6487,#6488,#6489,#6490,#6491)) ;
#2195 = EDGE_LOOP('',(#6492)) ;
#2196 = EDGE_LOOP('',(#6493)) ;
#2197 = EDGE_LOOP('',(#6494)) ;
#2198 = EDGE_LOOP('',(#6495)) ;
#2199 = EDGE_LOOP('',(#6496)) ;
#2200 = EDGE_LOOP('',(#6497,#6498,#6499,#6500)) ;
#2201 = EDGE_LOOP('',(#6501,#6502,#6503,#6504)) ;
#2202 = EDGE_LOOP('',(#6505,#6506,#6507,#6508)) ;
#2203 = EDGE_LOOP('',(#6509)) ;
#2204 = EDGE_LOOP('',(#6510)) ;
#2205 = EDGE_LOOP('',(#6511,#6512,#6513,#6514)) ;
#2206 = EDGE_LOOP('',(#6515,#6516,#6517,#6518)) ;
#2207 = EDGE_LOOP('',(#6519,#6520,#6521,#6522)) ;
#2208 = EDGE_LOOP('',(#6523,#6524,#6525,#6526)) ;
#2209 = EDGE_LOOP('',(#6527,#6528,#6529,#6530)) ;
#2210 = EDGE_LOOP('',(#6531,#6532,#6533,#6534)) ;
#2211 = EDGE_LOOP('',(#6535)) ;
#2212 = EDGE_LOOP('',(#6536,#6537,#6538,#6539)) ;
#2213 = EDGE_LOOP('',(#6540,#6541,#6542,#6543)) ;
#2214 = EDGE_LOOP('',(#6544,#6545,#6546,#6547)) ;
#2215 = EDGE_LOOP('',(#6548)) ;
#2216 = EDGE_LOOP('',(#6549,#6550,#6551,#6552)) ;
#2217 = EDGE_LOOP('',(#6553,#6554,#6555,#6556)) ;
#2218 = EDGE_LOOP('',(#6557,#6558,#6559,#6560)) ;
#2219 = EDGE_LOOP('',(#6561,#6562,#6563,#6564)) ;
#2220 = EDGE_LOOP('',(#6565,#6566)) ;
#2221 = EDGE_LOOP('',(#6567,#6568,#6569)) ;
#2222 = EDGE_LOOP('',(#6570,#6571,#6572,#6573)) ;
#2223 = EDGE_LOOP('',(#6574,#6575,#6576,#6577)) ;
#2224 = EDGE_LOOP('',(#6578,#6579,#6580,#6581)) ;
#2225 = EDGE_LOOP('',(#6582,#6583,#6584)) ;
#2226 = EDGE_LOOP('',(#6585,#6586)) ;
#2227 = EDGE_LOOP('',(#6587,#6588)) ;
#2228 = EDGE_LOOP('',(#6589,#6590)) ;
#2229 = EDGE_LOOP('',(#6591,#6592,#6593)) ;
#2230 = EDGE_LOOP('',(#6594,#6595,#6596,#6597)) ;
#2231 = EDGE_LOOP('',(#6598,#6599,#6600,#6601)) ;
#2232 = EDGE_LOOP('',(#6602,#6603,#6604,#6605)) ;
#2233 = EDGE_LOOP('',(#6606,#6607,#6608)) ;
#2234 = EDGE_LOOP('',(#6609,#6610)) ;
#2235 = EDGE_LOOP('',(#6611,#6612)) ;
#2236 = EDGE_LOOP('',(#6613,#6614)) ;
#2237 = EDGE_LOOP('',(#6615,#6616,#6617)) ;
#2238 = EDGE_LOOP('',(#6618,#6619,#6620,#6621)) ;
#2239 = EDGE_LOOP('',(#6622,#6623,#6624,#6625)) ;
#2240 = EDGE_LOOP('',(#6626,#6627,#6628,#6629)) ;
#2241 = EDGE_LOOP('',(#6630,#6631,#6632)) ;
#2242 = EDGE_LOOP('',(#6633,#6634)) ;
#2243 = EDGE_LOOP('',(#6635,#6636,#6637,#6638,#6639,#6640,#6641)) ;
#2244 = EDGE_LOOP('',(#6642)) ;
#2245 = EDGE_LOOP('',(#6643,#6644,#6645,#6646,#6647,#6648,#6649,#6650,#6651)) ;
#2246 = EDGE_LOOP('',(#6652,#6653,#6654,#6655,#6656,#6657,#6658,#6659,#6660)) ;
#2247 = EDGE_LOOP('',(#6661,#6662,#6663,#6664,#6665,#6666,#6667,#6668)) ;
#2248 = EDGE_LOOP('',(#6669,#6670,#6671,#6672,#6673,#6674,#6675,#6676)) ;
#2249 = EDGE_LOOP('',(#6677,#6678,#6679,#6680,#6681,#6682,#6683,#6684,#6685)) ;
#2250 = EDGE_LOOP('',(#6686,#6687,#6688,#6689,#6690,#6691,#6692,#6693,#6694)) ;
#2251 = EDGE_LOOP('',(#6695,#6696,#6697,#6698,#6699,#6700,#6701,#6702,#6703)) ;
#2252 = EDGE_LOOP('',(#6704,#6705,#6706,#6707,#6708,#6709,#6710,#6711,#6712)) ;
#2253 = EDGE_LOOP('',(#6713,#6714,#6715,#6716,#6717,#6718,#6719,#6720,#6721)) ;
#2254 = EDGE_LOOP('',(#6722,#6723,#6724,#6725,#6726,#6727,#6728,#6729,#6730)) ;
#2255 = EDGE_LOOP('',(#6731,#6732,#6733,#6734,#6735,#6736,#6737,#6738)) ;
#2256 = EDGE_LOOP('',(#6739,#6740,#6741,#6742,#6743,#6744,#6745,#6746)) ;
#2257 = EDGE_LOOP('',(#6747,#6748,#6749,#6750,#6751,#6752,#6753,#6754,#6755)) ;
#2258 = EDGE_LOOP('',(#6756,#6757,#6758,#6759,#6760,#6761,#6762,#6763,#6764)) ;
#2259 = EDGE_LOOP('',(#6765,#6766,#6767,#6768,#6769,#6770,#6771,#6772,#6773)) ;
#2260 = EDGE_LOOP('',(#6774,#6775,#6776,#6777,#6778,#6779,#6780,#6781,#6782)) ;
#2261 = EDGE_LOOP('',(#6783,#6784,#6785,#6786,#6787,#6788,#6789,#6790,#6791)) ;
#2262 = EDGE_LOOP('',(#6792,#6793,#6794,#6795,#6796,#6797,#6798,#6799,#6800)) ;
#2263 = EDGE_LOOP('',(#6801,#6802,#6803,#6804,#6805,#6806,#6807,#6808)) ;
#2264 = EDGE_LOOP('',(#6809,#6810,#6811,#6812,#6813,#6814,#6815,#6816)) ;
#2265 = EDGE_LOOP('',(#6817,#6818,#6819,#6820,#6821,#6822,#6823,#6824,#6825)) ;
#2266 = EDGE_LOOP('',(#6826,#6827,#6828,#6829,#6830,#6831,#6832,#6833,#6834)) ;
#2267 = EDGE_LOOP('',(#6835,#6836,#6837,#6838,#6839,#6840,#6841)) ;
#2268 = EDGE_LOOP('',(#6842)) ;
#2269 = EDGE_LOOP('',(#6843,#6844,#6845,#6846)) ;
#2270 = EDGE_LOOP('',(#6847)) ;
#2271 = EDGE_LOOP('',(#6848,#6849,#6850,#6851)) ;
#2272 = EDGE_LOOP('',(#6852)) ;
#2273 = EDGE_LOOP('',(#6853,#6854,#6855,#6856)) ;
#2274 = EDGE_LOOP('',(#6857,#6858,#6859,#6860)) ;
#2275 = EDGE_LOOP('',(#6861,#6862,#6863,#6864)) ;
#2276 = EDGE_LOOP('',(#6865,#6866,#6867,#6868)) ;
#2277 = EDGE_LOOP('',(#6869,#6870,#6871,#6872)) ;
#2278 = EDGE_LOOP('',(#6873,#6874,#6875,#6876)) ;
#2279 = EDGE_LOOP('',(#6877)) ;
#2280 = EDGE_LOOP('',(#6878)) ;
#2281 = EDGE_LOOP('',(#6879,#6880,#6881,#6882)) ;
#2282 = EDGE_LOOP('',(#6883)) ;
#2283 = EDGE_LOOP('',(#6884)) ;
#2284 = EDGE_LOOP('',(#6885,#6886,#6887,#6888)) ;
#2285 = EDGE_LOOP('',(#6889)) ;
#2286 = EDGE_LOOP('',(#6890)) ;
#2287 = EDGE_LOOP('',(#6891,#6892,#6893,#6894)) ;
#2288 = EDGE_LOOP('',(#6895)) ;
#2289 = EDGE_LOOP('',(#6896)) ;
#2290 = EDGE_LOOP('',(#6897,#6898)) ;
#2291 = EDGE_LOOP('',(#6899,#6900,#6901)) ;
#2292 = EDGE_LOOP('',(#6902,#6903,#6904,#6905)) ;
#2293 = EDGE_LOOP('',(#6906,#6907,#6908,#6909)) ;
#2294 = EDGE_LOOP('',(#6910,#6911,#6912,#6913)) ;
#2295 = EDGE_LOOP('',(#6914,#6915,#6916)) ;
#2296 = EDGE_LOOP('',(#6917,#6918)) ;
#2297 = EDGE_LOOP('',(#6919,#6920)) ;
#2298 = EDGE_LOOP('',(#6921,#6922)) ;
#2299 = EDGE_LOOP('',(#6923,#6924,#6925)) ;
#2300 = EDGE_LOOP('',(#6926,#6927,#6928,#6929)) ;
#2301 = EDGE_LOOP('',(#6930,#6931,#6932,#6933)) ;
#2302 = EDGE_LOOP('',(#6934,#6935,#6936,#6937)) ;
#2303 = EDGE_LOOP('',(#6938,#6939,#6940)) ;
#2304 = EDGE_LOOP('',(#6941,#6942)) ;
#2305 = EDGE_LOOP('',(#6943,#6944)) ;
#2306 = EDGE_LOOP('',(#6945,#6946)) ;
#2307 = EDGE_LOOP('',(#6947,#6948,#6949)) ;
#2308 = EDGE_LOOP('',(#6950,#6951,#6952,#6953)) ;
#2309 = EDGE_LOOP('',(#6954,#6955,#6956,#6957)) ;
#2310 = EDGE_LOOP('',(#6958,#6959,#6960,#6961)) ;
#2311 = EDGE_LOOP('',(#6962,#6963,#6964)) ;
#2312 = EDGE_LOOP('',(#6965,#6966)) ;
#2313 = EDGE_LOOP('',(#6967,#6968)) ;
#2314 = EDGE_LOOP('',(#6969,#6970)) ;
#2315 = EDGE_LOOP('',(#6971,#6972,#6973)) ;
#2316 = EDGE_LOOP('',(#6974,#6975,#6976,#6977)) ;
#2317 = EDGE_LOOP('',(#6978,#6979,#6980,#6981)) ;
#2318 = EDGE_LOOP('',(#6982,#6983,#6984,#6985)) ;
#2319 = EDGE_LOOP('',(#6986,#6987,#6988)) ;
#2320 = EDGE_LOOP('',(#6989,#6990)) ;
#2321 = EDGE_LOOP('',(#6991,#6992,#6993,#6994,#6995,#6996,#6997)) ;
#2322 = EDGE_LOOP('',(#6998)) ;
#2323 = EDGE_LOOP('',(#6999,#7000,#7001,#7002,#7003,#7004,#7005,#7006,#7007)) ;
#2324 = EDGE_LOOP('',(#7008,#7009,#7010,#7011,#7012,#7013,#7014,#7015,#7016)) ;
#2325 = EDGE_LOOP('',(#7017,#7018,#7019,#7020,#7021,#7022,#7023,#7024)) ;
#2326 = EDGE_LOOP('',(#7025,#7026,#7027,#7028,#7029,#7030,#7031,#7032)) ;
#2327 = EDGE_LOOP('',(#7033,#7034,#7035,#7036,#7037,#7038,#7039,#7040,#7041)) ;
#2328 = EDGE_LOOP('',(#7042,#7043,#7044,#7045,#7046,#7047,#7048,#7049,#7050)) ;
#2329 = EDGE_LOOP('',(#7051,#7052,#7053,#7054,#7055,#7056,#7057,#7058,#7059)) ;
#2330 = EDGE_LOOP('',(#7060,#7061,#7062,#7063,#7064,#7065,#7066,#7067,#7068)) ;
#2331 = EDGE_LOOP('',(#7069,#7070,#7071,#7072,#7073,#7074,#7075,#7076,#7077)) ;
#2332 = EDGE_LOOP('',(#7078,#7079,#7080,#7081,#7082,#7083,#7084,#7085,#7086)) ;
#2333 = EDGE_LOOP('',(#7087,#7088,#7089,#7090,#7091,#7092,#7093,#7094)) ;
#2334 = EDGE_LOOP('',(#7095,#7096,#7097,#7098,#7099,#7100,#7101,#7102)) ;
#2335 = EDGE_LOOP('',(#7103,#7104,#7105,#7106,#7107,#7108,#7109,#7110,#7111)) ;
#2336 = EDGE_LOOP('',(#7112,#7113,#7114,#7115,#7116,#7117,#7118,#7119,#7120)) ;
#2337 = EDGE_LOOP('',(#7121,#7122,#7123,#7124,#7125,#7126,#7127,#7128,#7129)) ;
#2338 = EDGE_LOOP('',(#7130,#7131,#7132,#7133,#7134,#7135,#7136,#7137,#7138)) ;
#2339 = EDGE_LOOP('',(#7139,#7140,#7141,#7142,#7143,#7144,#7145,#7146,#7147)) ;
#2340 = EDGE_LOOP('',(#7148,#7149,#7150,#7151,#7152,#7153,#7154,#7155,#7156)) ;
#2341 = EDGE_LOOP('',(#7157,#7158,#7159,#7160,#7161,#7162,#7163,#7164)) ;
#2342 = EDGE_LOOP('',(#7165,#7166,#7167,#7168,#7169,#7170,#7171,#7172)) ;
#2343 = EDGE_LOOP('',(#7173,#7174,#7175,#7176,#7177,#7178,#7179,#7180,#7181)) ;
#2344 = EDGE_LOOP('',(#7182,#7183,#7184,#7185,#7186,#7187,#7188,#7189,#7190)) ;
#2345 = EDGE_LOOP('',(#7191,#7192,#7193,#7194,#7195,#7196,#7197,#7198,#7199)) ;
#2346 = EDGE_LOOP('',(#7200,#7201,#7202,#7203,#7204,#7205,#7206,#7207,#7208)) ;
#2347 = EDGE_LOOP('',(#7209,#7210,#7211,#7212,#7213,#7214,#7215,#7216,#7217)) ;
#2348 = EDGE_LOOP('',(#7218,#7219,#7220,#7221,#7222,#7223,#7224,#7225,#7226)) ;
#2349 = EDGE_LOOP('',(#7227,#7228,#7229,#7230,#7231,#7232,#7233,#7234)) ;
#2350 = EDGE_LOOP('',(#7235,#7236,#7237,#7238,#7239,#7240,#7241,#7242)) ;
#2351 = EDGE_LOOP('',(#7243,#7244,#7245,#7246,#7247,#7248,#7249,#7250,#7251)) ;
#2352 = EDGE_LOOP('',(#7252,#7253,#7254,#7255,#7256,#7257,#7258,#7259,#7260)) ;
#2353 = EDGE_LOOP('',(#7261,#7262,#7263,#7264,#7265,#7266,#7267)) ;
#2354 = EDGE_LOOP('',(#7268)) ;
#2355 = EDGE_LOOP('',(#7269,#7270,#7271,#7272)) ;
#2356 = EDGE_LOOP('',(#7273,#7274,#7275,#7276)) ;
#2357 = EDGE_LOOP('',(#7277)) ;
#2358 = EDGE_LOOP('',(#7278,#7279,#7280,#7281)) ;
#2359 = EDGE_LOOP('',(#7282,#7283,#7284,#7285)) ;
#2360 = EDGE_LOOP('',(#7286)) ;
#2361 = EDGE_LOOP('',(#7287,#7288,#7289,#7290)) ;
#2362 = EDGE_LOOP('',(#7291,#7292,#7293,#7294)) ;
#2363 = EDGE_LOOP('',(#7295,#7296,#7297,#7298)) ;
#2364 = EDGE_LOOP('',(#7299,#7300,#7301,#7302,#7303,#7304,#7305,#7306)) ;
#2365 = EDGE_LOOP('',(#7307,#7308,#7309,#7310)) ;
#2366 = EDGE_LOOP('',(#7311,#7312,#7313,#7314,#7315,#7316,#7317,#7318)) ;
#2367 = EDGE_LOOP('',(#7319,#7320,#7321,#7322)) ;
#2368 = EDGE_LOOP('',(#7323,#7324,#7325,#7326)) ;
#2369 = EDGE_LOOP('',(#7327,#7328,#7329,#7330)) ;
#2370 = EDGE_LOOP('',(#7331,#7332,#7333,#7334)) ;
#2371 = EDGE_LOOP('',(#7335,#7336,#7337,#7338)) ;
#2372 = EDGE_LOOP('',(#7339,#7340,#7341,#7342)) ;
#2373 = EDGE_LOOP('',(#7343)) ;
#2374 = EDGE_LOOP('',(#7344,#7345,#7346,#7347)) ;
#2375 = EDGE_LOOP('',(#7348,#7349,#7350,#7351)) ;
#2376 = EDGE_LOOP('',(#7352,#7353,#7354,#7355)) ;
#2377 = EDGE_LOOP('',(#7356,#7357,#7358,#7359)) ;
#2378 = EDGE_LOOP('',(#7360,#7361,#7362,#7363)) ;
#2379 = EDGE_LOOP('',(#7364,#7365,#7366,#7367)) ;
#2380 = EDGE_LOOP('',(#7368,#7369,#7370,#7371)) ;
#2381 = EDGE_LOOP('',(#7372,#7373,#7374,#7375)) ;
#2382 = EDGE_LOOP('',(#7376)) ;
#2383 = EDGE_LOOP('',(#7377,#7378)) ;
#2384 = EDGE_LOOP('',(#7379,#7380)) ;
#2385 = EDGE_LOOP('',(#7381,#7382,#7383,#7384,#7385)) ;
#2386 = EDGE_LOOP('',(#7386)) ;
#2387 = EDGE_LOOP('',(#7387,#7388,#7389,#7390)) ;
#2388 = EDGE_LOOP('',(#7391)) ;
#2389 = EDGE_LOOP('',(#7392)) ;
#2390 = EDGE_LOOP('',(#7393,#7394,#7395,#7396)) ;
#2391 = EDGE_LOOP('',(#7397)) ;
#2392 = EDGE_LOOP('',(#7398)) ;
#2393 = EDGE_LOOP('',(#7399,#7400,#7401,#7402)) ;
#2394 = EDGE_LOOP('',(#7403)) ;
#2395 = EDGE_LOOP('',(#7404)) ;
#2396 = EDGE_LOOP('',(#7405,#7406,#7407,#7408)) ;
#2397 = EDGE_LOOP('',(#7409)) ;
#2398 = EDGE_LOOP('',(#7410)) ;
#2399 = EDGE_LOOP('',(#7411,#7412,#7413,#7414)) ;
#2400 = EDGE_LOOP('',(#7415)) ;
#2401 = EDGE_LOOP('',(#7416)) ;
#2402 = EDGE_LOOP('',(#7417,#7418,#7419,#7420,#7421,#7422,#7423)) ;
#2403 = EDGE_LOOP('',(#7424,#7425,#7426,#7427)) ;
#2404 = EDGE_LOOP('',(#7428,#7429,#7430,#7431)) ;
#2405 = EDGE_LOOP('',(#7432,#7433,#7434,#7435,#7436,#7437,#7438)) ;
#2406 = EDGE_LOOP('',(#7439,#7440,#7441,#7442,#7443,#7444,#7445,#7446)) ;
#2407 = EDGE_LOOP('',(#7447,#7448,#7449,#7450)) ;
#2408 = EDGE_LOOP('',(#7451,#7452,#7453,#7454)) ;
#2409 = EDGE_LOOP('',(#7455,#7456,#7457,#7458,#7459,#7460,#7461,#7462,#7463,
#7464,#7465,#7466)) ;
#2410 = EDGE_LOOP('',(#7467,#7468,#7469,#7470)) ;
#2411 = EDGE_LOOP('',(#7471,#7472,#7473,#7474,#7475,#7476,#7477,#7478)) ;
#2412 = EDGE_LOOP('',(#7479,#7480,#7481,#7482)) ;
#2413 = EDGE_LOOP('',(#7483)) ;
#2414 = EDGE_LOOP('',(#7484,#7485,#7486,#7487)) ;
#2415 = EDGE_LOOP('',(#7488)) ;
#2416 = EDGE_LOOP('',(#7489,#7490,#7491,#7492)) ;
#2417 = EDGE_LOOP('',(#7493)) ;
#2418 = EDGE_LOOP('',(#7494)) ;
#2419 = EDGE_LOOP('',(#7495,#7496,#7497,#7498)) ;
#2420 = EDGE_LOOP('',(#7499)) ;
#2421 = EDGE_LOOP('',(#7500)) ;
#2422 = EDGE_LOOP('',(#7501,#7502,#7503,#7504)) ;
#2423 = EDGE_LOOP('',(#7505)) ;
#2424 = EDGE_LOOP('',(#7506)) ;
#2425 = EDGE_LOOP('',(#7507,#7508,#7509,#7510)) ;
#2426 = EDGE_LOOP('',(#7511)) ;
#2427 = EDGE_LOOP('',(#7512)) ;
#2428 = EDGE_LOOP('',(#7513,#7514,#7515,#7516)) ;
#2429 = EDGE_LOOP('',(#7517)) ;
#2430 = EDGE_LOOP('',(#7518,#7519,#7520,#7521)) ;
#2431 = EDGE_LOOP('',(#7522)) ;
#2432 = EDGE_LOOP('',(#7523)) ;
#2433 = EDGE_LOOP('',(#7524)) ;
#2434 = EDGE_LOOP('',(#7525,#7526,#7527,#7528)) ;
#2435 = EDGE_LOOP('',(#7529)) ;
#2436 = EDGE_LOOP('',(#7530,#7531,#7532,#7533)) ;
#2437 = EDGE_LOOP('',(#7534)) ;
#2438 = EDGE_LOOP('',(#7535)) ;
#2439 = EDGE_LOOP('',(#7536)) ;
#2440 = LINE('',#12891,#2914) ;
#2441 = LINE('',#12893,#2915) ;
#2442 = LINE('',#12895,#2916) ;
#2443 = LINE('',#12896,#2917) ;
#2444 = LINE('',#12899,#2918) ;
#2445 = LINE('',#12901,#2919) ;
#2446 = LINE('',#12903,#2920) ;
#2447 = LINE('',#12905,#2921) ;
#2448 = LINE('',#12906,#2922) ;
#2449 = LINE('',#12909,#2923) ;
#2450 = LINE('',#12911,#2924) ;
#2451 = LINE('',#12913,#2925) ;
#2452 = LINE('',#12914,#2926) ;
#2453 = LINE('',#12917,#2927) ;
#2454 = LINE('',#12918,#2928) ;
#2455 = LINE('',#12920,#2929) ;
#2456 = LINE('',#12923,#2930) ;
#2457 = LINE('',#12924,#2931) ;
#2458 = LINE('',#12931,#2932) ;
#2459 = LINE('',#12933,#2933) ;
#2460 = LINE('',#12935,#2934) ;
#2461 = LINE('',#12936,#2935) ;
#2462 = LINE('',#12939,#2936) ;
#2463 = LINE('',#12941,#2937) ;
#2464 = LINE('',#12943,#2938) ;
#2465 = LINE('',#12944,#2939) ;
#2466 = LINE('',#12953,#2940) ;
#2467 = LINE('',#12960,#2941) ;
#2468 = LINE('',#12967,#2942) ;
#2469 = LINE('',#12972,#2943) ;
#2470 = LINE('',#12974,#2944) ;
#2471 = LINE('',#12976,#2945) ;
#2472 = LINE('',#12977,#2946) ;
#2473 = LINE('',#12980,#2947) ;
#2474 = LINE('',#12982,#2948) ;
#2475 = LINE('',#12983,#2949) ;
#2476 = LINE('',#12986,#2950) ;
#2477 = LINE('',#12987,#2951) ;
#2478 = LINE('',#12990,#2952) ;
#2479 = LINE('',#12991,#2953) ;
#2480 = LINE('',#12994,#2954) ;
#2481 = LINE('',#12996,#2955) ;
#2482 = LINE('',#12998,#2956) ;
#2483 = LINE('',#13000,#2957) ;
#2484 = LINE('',#13001,#2958) ;
#2485 = LINE('',#13006,#2959) ;
#2486 = LINE('',#13011,#2960) ;
#2487 = LINE('',#13013,#2961) ;
#2488 = LINE('',#13015,#2962) ;
#2489 = LINE('',#13016,#2963) ;
#2490 = LINE('',#13019,#2964) ;
#2491 = LINE('',#13021,#2965) ;
#2492 = LINE('',#13022,#2966) ;
#2493 = LINE('',#13025,#2967) ;
#2494 = LINE('',#13026,#2968) ;
#2495 = LINE('',#13029,#2969) ;
#2496 = LINE('',#13030,#2970) ;
#2497 = LINE('',#13033,#2971) ;
#2498 = LINE('',#13035,#2972) ;
#2499 = LINE('',#13037,#2973) ;
#2500 = LINE('',#13039,#2974) ;
#2501 = LINE('',#13040,#2975) ;
#2502 = LINE('',#13045,#2976) ;
#2503 = LINE('',#13050,#2977) ;
#2504 = LINE('',#13057,#2978) ;
#2505 = LINE('',#13062,#2979) ;
#2506 = LINE('',#13068,#2980) ;
#2507 = LINE('',#13073,#2981) ;
#2508 = LINE('',#13080,#2982) ;
#2509 = LINE('',#13086,#2983) ;
#2510 = LINE('',#13091,#2984) ;
#2511 = LINE('',#13093,#2985) ;
#2512 = LINE('',#13095,#2986) ;
#2513 = LINE('',#13096,#2987) ;
#2514 = LINE('',#13098,#2988) ;
#2515 = LINE('',#13099,#2989) ;
#2516 = LINE('',#13101,#2990) ;
#2517 = LINE('',#13103,#2991) ;
#2518 = LINE('',#13108,#2992) ;
#2519 = LINE('',#13110,#2993) ;
#2520 = LINE('',#13112,#2994) ;
#2521 = LINE('',#13113,#2995) ;
#2522 = LINE('',#13115,#2996) ;
#2523 = LINE('',#13116,#2997) ;
#2524 = LINE('',#13118,#2998) ;
#2525 = LINE('',#13120,#2999) ;
#2526 = LINE('',#13125,#3000) ;
#2527 = LINE('',#13128,#3001) ;
#2528 = LINE('',#13129,#3002) ;
#2529 = LINE('',#13131,#3003) ;
#2530 = LINE('',#13134,#3004) ;
#2531 = LINE('',#13135,#3005) ;
#2532 = LINE('',#13137,#3006) ;
#2533 = LINE('',#13138,#3007) ;
#2534 = LINE('',#13145,#3008) ;
#2535 = LINE('',#13149,#3009) ;
#2536 = LINE('',#13153,#3010) ;
#2537 = LINE('',#13156,#3011) ;
#2538 = LINE('',#13161,#3012) ;
#2539 = LINE('',#13164,#3013) ;
#2540 = LINE('',#13167,#3014) ;
#2541 = LINE('',#13169,#3015) ;
#2542 = LINE('',#13171,#3016) ;
#2543 = LINE('',#13173,#3017) ;
#2544 = LINE('',#13174,#3018) ;
#2545 = LINE('',#13178,#3019) ;
#2546 = LINE('',#13181,#3020) ;
#2547 = LINE('',#13186,#3021) ;
#2548 = LINE('',#13190,#3022) ;
#2549 = LINE('',#13195,#3023) ;
#2550 = LINE('',#13199,#3024) ;
#2551 = LINE('',#13202,#3025) ;
#2552 = LINE('',#13203,#3026) ;
#2553 = LINE('',#13207,#3027) ;
#2554 = LINE('',#13209,#3028) ;
#2555 = LINE('',#13211,#3029) ;
#2556 = LINE('',#13212,#3030) ;
#2557 = LINE('',#13214,#3031) ;
#2558 = LINE('',#13217,#3032) ;
#2559 = LINE('',#13218,#3033) ;
#2560 = LINE('',#13221,#3034) ;
#2561 = LINE('',#13226,#3035) ;
#2562 = LINE('',#13229,#3036) ;
#2563 = LINE('',#13230,#3037) ;
#2564 = LINE('',#13232,#3038) ;
#2565 = LINE('',#13242,#3039) ;
#2566 = LINE('',#13248,#3040) ;
#2567 = LINE('',#13250,#3041) ;
#2568 = LINE('',#13252,#3042) ;
#2569 = LINE('',#13253,#3043) ;
#2570 = LINE('',#13256,#3044) ;
#2571 = LINE('',#13258,#3045) ;
#2572 = LINE('',#13259,#3046) ;
#2573 = LINE('',#13262,#3047) ;
#2574 = LINE('',#13263,#3048) ;
#2575 = LINE('',#13266,#3049) ;
#2576 = LINE('',#13267,#3050) ;
#2577 = LINE('',#13269,#3051) ;
#2578 = LINE('',#13273,#3052) ;
#2579 = LINE('',#13275,#3053) ;
#2580 = LINE('',#13277,#3054) ;
#2581 = LINE('',#13278,#3055) ;
#2582 = LINE('',#13281,#3056) ;
#2583 = LINE('',#13283,#3057) ;
#2584 = LINE('',#13284,#3058) ;
#2585 = LINE('',#13287,#3059) ;
#2586 = LINE('',#13288,#3060) ;
#2587 = LINE('',#13291,#3061) ;
#2588 = LINE('',#13292,#3062) ;
#2589 = LINE('',#13294,#3063) ;
#2590 = LINE('',#13298,#3064) ;
#2591 = LINE('',#13300,#3065) ;
#2592 = LINE('',#13302,#3066) ;
#2593 = LINE('',#13303,#3067) ;
#2594 = LINE('',#13306,#3068) ;
#2595 = LINE('',#13308,#3069) ;
#2596 = LINE('',#13309,#3070) ;
#2597 = LINE('',#13312,#3071) ;
#2598 = LINE('',#13313,#3072) ;
#2599 = LINE('',#13316,#3073) ;
#2600 = LINE('',#13317,#3074) ;
#2601 = LINE('',#13319,#3075) ;
#2602 = LINE('',#13324,#3076) ;
#2603 = LINE('',#13330,#3077) ;
#2604 = LINE('',#13339,#3078) ;
#2605 = LINE('',#13344,#3079) ;
#2606 = LINE('',#13353,#3080) ;
#2607 = LINE('',#13361,#3081) ;
#2608 = LINE('',#13367,#3082) ;
#2609 = LINE('',#13376,#3083) ;
#2610 = LINE('',#13382,#3084) ;
#2611 = LINE('',#13395,#3085) ;
#2612 = LINE('',#13407,#3086) ;
#2613 = LINE('',#13413,#3087) ;
#2614 = LINE('',#13420,#3088) ;
#2615 = LINE('',#13429,#3089) ;
#2616 = LINE('',#13436,#3090) ;
#2617 = LINE('',#13445,#3091) ;
#2618 = LINE('',#13453,#3092) ;
#2619 = LINE('',#13455,#3093) ;
#2620 = LINE('',#13457,#3094) ;
#2621 = LINE('',#13458,#3095) ;
#2622 = LINE('',#13464,#3096) ;
#2623 = LINE('',#13465,#3097) ;
#2624 = LINE('',#13468,#3098) ;
#2625 = LINE('',#13470,#3099) ;
#2626 = LINE('',#13471,#3100) ;
#2627 = LINE('',#13475,#3101) ;
#2628 = LINE('',#13479,#3102) ;
#2629 = LINE('',#13483,#3103) ;
#2630 = LINE('',#13485,#3104) ;
#2631 = LINE('',#13487,#3105) ;
#2632 = LINE('',#13492,#3106) ;
#2633 = LINE('',#13501,#3107) ;
#2634 = LINE('',#13505,#3108) ;
#2635 = LINE('',#13509,#3109) ;
#2636 = LINE('',#13514,#3110) ;
#2637 = LINE('',#13523,#3111) ;
#2638 = LINE('',#13576,#3112) ;
#2639 = LINE('',#13611,#3113) ;
#2640 = LINE('',#13617,#3114) ;
#2641 = LINE('',#13621,#3115) ;
#2642 = LINE('',#13632,#3116) ;
#2643 = LINE('',#13638,#3117) ;
#2644 = LINE('',#13647,#3118) ;
#2645 = LINE('',#13653,#3119) ;
#2646 = LINE('',#13660,#3120) ;
#2647 = LINE('',#13669,#3121) ;
#2648 = LINE('',#13678,#3122) ;
#2649 = LINE('',#13697,#3123) ;
#2650 = LINE('',#13702,#3124) ;
#2651 = LINE('',#13704,#3125) ;
#2652 = LINE('',#13706,#3126) ;
#2653 = LINE('',#13707,#3127) ;
#2654 = LINE('',#13710,#3128) ;
#2655 = LINE('',#13712,#3129) ;
#2656 = LINE('',#13713,#3130) ;
#2657 = LINE('',#13717,#3131) ;
#2658 = LINE('',#13718,#3132) ;
#2659 = LINE('',#13719,#3133) ;
#2660 = LINE('',#13722,#3134) ;
#2661 = LINE('',#13726,#3135) ;
#2662 = LINE('',#13728,#3136) ;
#2663 = LINE('',#13730,#3137) ;
#2664 = LINE('',#13733,#3138) ;
#2665 = LINE('',#13738,#3139) ;
#2666 = LINE('',#13739,#3140) ;
#2667 = LINE('',#13742,#3141) ;
#2668 = LINE('',#13747,#3142) ;
#2669 = LINE('',#13750,#3143) ;
#2670 = LINE('',#13752,#3144) ;
#2671 = LINE('',#13756,#3145) ;
#2672 = LINE('',#13757,#3146) ;
#2673 = LINE('',#13759,#3147) ;
#2674 = LINE('',#13762,#3148) ;
#2675 = LINE('',#13763,#3149) ;
#2676 = LINE('',#13765,#3150) ;
#2677 = LINE('',#13775,#3151) ;
#2678 = LINE('',#13781,#3152) ;
#2679 = LINE('',#14063,#3153) ;
#2680 = LINE('',#14071,#3154) ;
#2681 = LINE('',#14075,#3155) ;
#2682 = LINE('',#14078,#3156) ;
#2683 = LINE('',#14081,#3157) ;
#2684 = LINE('',#14084,#3158) ;
#2685 = LINE('',#14090,#3159) ;
#2686 = LINE('',#14097,#3160) ;
#2687 = LINE('',#14102,#3161) ;
#2688 = LINE('',#14109,#3162) ;
#2689 = LINE('',#14113,#3163) ;
#2690 = LINE('',#14116,#3164) ;
#2691 = LINE('',#14119,#3165) ;
#2692 = LINE('',#14122,#3166) ;
#2693 = LINE('',#14128,#3167) ;
#2694 = LINE('',#14135,#3168) ;
#2695 = LINE('',#14140,#3169) ;
#2696 = LINE('',#14147,#3170) ;
#2697 = LINE('',#14151,#3171) ;
#2698 = LINE('',#14154,#3172) ;
#2699 = LINE('',#14157,#3173) ;
#2700 = LINE('',#14160,#3174) ;
#2701 = LINE('',#14166,#3175) ;
#2702 = LINE('',#14173,#3176) ;
#2703 = LINE('',#14178,#3177) ;
#2704 = LINE('',#14185,#3178) ;
#2705 = LINE('',#14189,#3179) ;
#2706 = LINE('',#14192,#3180) ;
#2707 = LINE('',#14195,#3181) ;
#2708 = LINE('',#14198,#3182) ;
#2709 = LINE('',#14204,#3183) ;
#2710 = LINE('',#14211,#3184) ;
#2711 = LINE('',#14216,#3185) ;
#2712 = LINE('',#14223,#3186) ;
#2713 = LINE('',#14227,#3187) ;
#2714 = LINE('',#14230,#3188) ;
#2715 = LINE('',#14233,#3189) ;
#2716 = LINE('',#14236,#3190) ;
#2717 = LINE('',#14242,#3191) ;
#2718 = LINE('',#14249,#3192) ;
#2719 = LINE('',#14264,#3193) ;
#2720 = LINE('',#14268,#3194) ;
#2721 = LINE('',#14271,#3195) ;
#2722 = LINE('',#14279,#3196) ;
#2723 = LINE('',#14281,#3197) ;
#2724 = LINE('',#14283,#3198) ;
#2725 = LINE('',#14284,#3199) ;
#2726 = LINE('',#14287,#3200) ;
#2727 = LINE('',#14289,#3201) ;
#2728 = LINE('',#14290,#3202) ;
#2729 = LINE('',#14293,#3203) ;
#2730 = LINE('',#14294,#3204) ;
#2731 = LINE('',#14297,#3205) ;
#2732 = LINE('',#14298,#3206) ;
#2733 = LINE('',#14300,#3207) ;
#2734 = LINE('',#14305,#3208) ;
#2735 = LINE('',#14311,#3209) ;
#2736 = LINE('',#14313,#3210) ;
#2737 = LINE('',#14315,#3211) ;
#2738 = LINE('',#14316,#3212) ;
#2739 = LINE('',#14320,#3213) ;
#2740 = LINE('',#14322,#3214) ;
#2741 = LINE('',#14324,#3215) ;
#2742 = LINE('',#14325,#3216) ;
#2743 = LINE('',#14327,#3217) ;
#2744 = LINE('',#14328,#3218) ;
#2745 = LINE('',#14330,#3219) ;
#2746 = LINE('',#14332,#3220) ;
#2747 = LINE('',#14502,#3221) ;
#2748 = LINE('',#14510,#3222) ;
#2749 = LINE('',#14514,#3223) ;
#2750 = LINE('',#14517,#3224) ;
#2751 = LINE('',#14520,#3225) ;
#2752 = LINE('',#14523,#3226) ;
#2753 = LINE('',#14529,#3227) ;
#2754 = LINE('',#14536,#3228) ;
#2755 = LINE('',#14541,#3229) ;
#2756 = LINE('',#14548,#3230) ;
#2757 = LINE('',#14552,#3231) ;
#2758 = LINE('',#14555,#3232) ;
#2759 = LINE('',#14558,#3233) ;
#2760 = LINE('',#14561,#3234) ;
#2761 = LINE('',#14567,#3235) ;
#2762 = LINE('',#14574,#3236) ;
#2763 = LINE('',#14579,#3237) ;
#2764 = LINE('',#14586,#3238) ;
#2765 = LINE('',#14590,#3239) ;
#2766 = LINE('',#14593,#3240) ;
#2767 = LINE('',#14596,#3241) ;
#2768 = LINE('',#14599,#3242) ;
#2769 = LINE('',#14605,#3243) ;
#2770 = LINE('',#14612,#3244) ;
#2771 = LINE('',#14620,#3245) ;
#2772 = LINE('',#14626,#3246) ;
#2773 = LINE('',#14628,#3247) ;
#2774 = LINE('',#14630,#3248) ;
#2775 = LINE('',#14631,#3249) ;
#2776 = LINE('',#14635,#3250) ;
#2777 = LINE('',#14637,#3251) ;
#2778 = LINE('',#14639,#3252) ;
#2779 = LINE('',#14640,#3253) ;
#2780 = LINE('',#14642,#3254) ;
#2781 = LINE('',#14643,#3255) ;
#2782 = LINE('',#14645,#3256) ;
#2783 = LINE('',#14647,#3257) ;
#2784 = LINE('',#14654,#3258) ;
#2785 = LINE('',#14662,#3259) ;
#2786 = LINE('',#14671,#3260) ;
#2787 = LINE('',#14680,#3261) ;
#2788 = LINE('',#14908,#3262) ;
#2789 = LINE('',#14916,#3263) ;
#2790 = LINE('',#14920,#3264) ;
#2791 = LINE('',#14923,#3265) ;
#2792 = LINE('',#14926,#3266) ;
#2793 = LINE('',#14929,#3267) ;
#2794 = LINE('',#14935,#3268) ;
#2795 = LINE('',#14942,#3269) ;
#2796 = LINE('',#14947,#3270) ;
#2797 = LINE('',#14954,#3271) ;
#2798 = LINE('',#14958,#3272) ;
#2799 = LINE('',#14961,#3273) ;
#2800 = LINE('',#14964,#3274) ;
#2801 = LINE('',#14967,#3275) ;
#2802 = LINE('',#14973,#3276) ;
#2803 = LINE('',#14980,#3277) ;
#2804 = LINE('',#14985,#3278) ;
#2805 = LINE('',#14992,#3279) ;
#2806 = LINE('',#14996,#3280) ;
#2807 = LINE('',#14999,#3281) ;
#2808 = LINE('',#15002,#3282) ;
#2809 = LINE('',#15005,#3283) ;
#2810 = LINE('',#15011,#3284) ;
#2811 = LINE('',#15018,#3285) ;
#2812 = LINE('',#15023,#3286) ;
#2813 = LINE('',#15030,#3287) ;
#2814 = LINE('',#15034,#3288) ;
#2815 = LINE('',#15037,#3289) ;
#2816 = LINE('',#15040,#3290) ;
#2817 = LINE('',#15043,#3291) ;
#2818 = LINE('',#15049,#3292) ;
#2819 = LINE('',#15056,#3293) ;
#2820 = LINE('',#15076,#3294) ;
#2821 = LINE('',#15081,#3295) ;
#2822 = LINE('',#15083,#3296) ;
#2823 = LINE('',#15085,#3297) ;
#2824 = LINE('',#15086,#3298) ;
#2825 = LINE('',#15090,#3299) ;
#2826 = LINE('',#15091,#3300) ;
#2827 = LINE('',#15092,#3301) ;
#2828 = LINE('',#15096,#3302) ;
#2829 = LINE('',#15097,#3303) ;
#2830 = LINE('',#15098,#3304) ;
#2831 = LINE('',#15102,#3305) ;
#2832 = LINE('',#15104,#3306) ;
#2833 = LINE('',#15106,#3307) ;
#2834 = LINE('',#15107,#3308) ;
#2835 = LINE('',#15110,#3309) ;
#2836 = LINE('',#15112,#3310) ;
#2837 = LINE('',#15113,#3311) ;
#2838 = LINE('',#15116,#3312) ;
#2839 = LINE('',#15118,#3313) ;
#2840 = LINE('',#15119,#3314) ;
#2841 = LINE('',#15121,#3315) ;
#2842 = LINE('',#15122,#3316) ;
#2843 = LINE('',#15124,#3317) ;
#2844 = LINE('',#15126,#3318) ;
#2845 = LINE('',#15132,#3319) ;
#2846 = LINE('',#15134,#3320) ;
#2847 = LINE('',#15136,#3321) ;
#2848 = LINE('',#15137,#3322) ;
#2849 = LINE('',#15140,#3323) ;
#2850 = LINE('',#15142,#3324) ;
#2851 = LINE('',#15143,#3325) ;
#2852 = LINE('',#15146,#3326) ;
#2853 = LINE('',#15148,#3327) ;
#2854 = LINE('',#15149,#3328) ;
#2855 = LINE('',#15151,#3329) ;
#2856 = LINE('',#15152,#3330) ;
#2857 = LINE('',#15158,#3331) ;
#2858 = LINE('',#15163,#3332) ;
#2859 = LINE('',#15165,#3333) ;
#2860 = LINE('',#15167,#3334) ;
#2861 = LINE('',#15168,#3335) ;
#2862 = LINE('',#15172,#3336) ;
#2863 = LINE('',#15174,#3337) ;
#2864 = LINE('',#15176,#3338) ;
#2865 = LINE('',#15177,#3339) ;
#2866 = LINE('',#15179,#3340) ;
#2867 = LINE('',#15180,#3341) ;
#2868 = LINE('',#15182,#3342) ;
#2869 = LINE('',#15184,#3343) ;
#2870 = LINE('',#15197,#3344) ;
#2871 = LINE('',#15203,#3345) ;
#2872 = LINE('',#15211,#3346) ;
#2873 = LINE('',#15220,#3347) ;
#2874 = LINE('',#15228,#3348) ;
#2875 = LINE('',#15236,#3349) ;
#2876 = LINE('',#15246,#3350) ;
#2877 = LINE('',#15248,#3351) ;
#2878 = LINE('',#15250,#3352) ;
#2879 = LINE('',#15252,#3353) ;
#2880 = LINE('',#15254,#3354) ;
#2881 = LINE('',#15258,#3355) ;
#2882 = LINE('',#15260,#3356) ;
#2883 = LINE('',#15261,#3357) ;
#2884 = LINE('',#15264,#3358) ;
#2885 = LINE('',#15266,#3359) ;
#2886 = LINE('',#15267,#3360) ;
#2887 = LINE('',#15272,#3361) ;
#2888 = LINE('',#15274,#3362) ;
#2889 = LINE('',#15275,#3363) ;
#2890 = LINE('',#15279,#3364) ;
#2891 = LINE('',#15281,#3365) ;
#2892 = LINE('',#15283,#3366) ;
#2893 = LINE('',#15285,#3367) ;
#2894 = LINE('',#15286,#3368) ;
#2895 = LINE('',#15289,#3369) ;
#2896 = LINE('',#15290,#3370) ;
#2897 = LINE('',#15293,#3371) ;
#2898 = LINE('',#15294,#3372) ;
#2899 = LINE('',#15298,#3373) ;
#2900 = LINE('',#15300,#3374) ;
#2901 = LINE('',#15304,#3375) ;
#2902 = LINE('',#15306,#3376) ;
#2903 = LINE('',#15307,#3377) ;
#2904 = LINE('',#15309,#3378) ;
#2905 = LINE('',#15310,#3379) ;
#2906 = LINE('',#15318,#3380) ;
#2907 = LINE('',#15326,#3381) ;
#2908 = LINE('',#15334,#3382) ;
#2909 = LINE('',#15343,#3383) ;
#2910 = LINE('',#15362,#3384) ;
#2911 = LINE('',#15369,#3385) ;
#2912 = LINE('',#15378,#3386) ;
#2913 = LINE('',#15385,#3387) ;
#2914 = VECTOR('',#9933,1.) ;
#2915 = VECTOR('',#9934,1.) ;
#2916 = VECTOR('',#9935,1.) ;
#2917 = VECTOR('',#9936,1.) ;
#2918 = VECTOR('',#9939,1.) ;
#2919 = VECTOR('',#9940,1.) ;
#2920 = VECTOR('',#9941,1.) ;
#2921 = VECTOR('',#9942,1.) ;
#2922 = VECTOR('',#9943,1.) ;
#2923 = VECTOR('',#9946,1.) ;
#2924 = VECTOR('',#9947,1.) ;
#2925 = VECTOR('',#9948,1.) ;
#2926 = VECTOR('',#9949,1.) ;
#2927 = VECTOR('',#9952,1.) ;
#2928 = VECTOR('',#9953,1.) ;
#2929 = VECTOR('',#9956,1.) ;
#2930 = VECTOR('',#9959,1.) ;
#2931 = VECTOR('',#9960,1.) ;
#2932 = VECTOR('',#9965,1.) ;
#2933 = VECTOR('',#9966,1.) ;
#2934 = VECTOR('',#9967,1.) ;
#2935 = VECTOR('',#9968,1.) ;
#2936 = VECTOR('',#9969,1.) ;
#2937 = VECTOR('',#9970,1.) ;
#2938 = VECTOR('',#9971,1.) ;
#2939 = VECTOR('',#9972,1.) ;
#2940 = VECTOR('',#9981,0.155) ;
#2941 = VECTOR('',#9990,0.155) ;
#2942 = VECTOR('',#9999,0.17) ;
#2943 = VECTOR('',#10004,1.) ;
#2944 = VECTOR('',#10005,1.) ;
#2945 = VECTOR('',#10006,1.) ;
#2946 = VECTOR('',#10007,1.) ;
#2947 = VECTOR('',#10010,1.) ;
#2948 = VECTOR('',#10011,1.) ;
#2949 = VECTOR('',#10012,1.) ;
#2950 = VECTOR('',#10015,1.) ;
#2951 = VECTOR('',#10016,1.) ;
#2952 = VECTOR('',#10019,1.) ;
#2953 = VECTOR('',#10020,1.) ;
#2954 = VECTOR('',#10023,1.) ;
#2955 = VECTOR('',#10024,1.) ;
#2956 = VECTOR('',#10025,1.) ;
#2957 = VECTOR('',#10026,1.) ;
#2958 = VECTOR('',#10027,1.) ;
#2959 = VECTOR('',#10032,0.17) ;
#2960 = VECTOR('',#10037,1.) ;
#2961 = VECTOR('',#10038,1.) ;
#2962 = VECTOR('',#10039,1.) ;
#2963 = VECTOR('',#10040,1.) ;
#2964 = VECTOR('',#10043,1.) ;
#2965 = VECTOR('',#10044,1.) ;
#2966 = VECTOR('',#10045,1.) ;
#2967 = VECTOR('',#10048,1.) ;
#2968 = VECTOR('',#10049,1.) ;
#2969 = VECTOR('',#10052,1.) ;
#2970 = VECTOR('',#10053,1.) ;
#2971 = VECTOR('',#10056,1.) ;
#2972 = VECTOR('',#10057,1.) ;
#2973 = VECTOR('',#10058,1.) ;
#2974 = VECTOR('',#10059,1.) ;
#2975 = VECTOR('',#10060,1.) ;
#2976 = VECTOR('',#10065,0.14) ;
#2977 = VECTOR('',#10072,0.4) ;
#2978 = VECTOR('',#10081,0.8) ;
#2979 = VECTOR('',#10088,1.) ;
#2980 = VECTOR('',#10095,0.21) ;
#2981 = VECTOR('',#10102,0.4) ;
#2982 = VECTOR('',#10111,0.13) ;
#2983 = VECTOR('',#10118,0.13) ;
#2984 = VECTOR('',#10123,1.) ;
#2985 = VECTOR('',#10124,1.) ;
#2986 = VECTOR('',#10125,1.) ;
#2987 = VECTOR('',#10126,1.) ;
#2988 = VECTOR('',#10129,1.) ;
#2989 = VECTOR('',#10130,1.) ;
#2990 = VECTOR('',#10133,1.) ;
#2991 = VECTOR('',#10136,1.) ;
#2992 = VECTOR('',#10141,1.) ;
#2993 = VECTOR('',#10142,1.) ;
#2994 = VECTOR('',#10143,1.) ;
#2995 = VECTOR('',#10144,1.) ;
#2996 = VECTOR('',#10147,1.) ;
#2997 = VECTOR('',#10148,1.) ;
#2998 = VECTOR('',#10151,1.) ;
#2999 = VECTOR('',#10154,1.) ;
#3000 = VECTOR('',#10161,1.31) ;
#3001 = VECTOR('',#10164,1.) ;
#3002 = VECTOR('',#10165,1.) ;
#3003 = VECTOR('',#10168,1.) ;
#3004 = VECTOR('',#10173,1.) ;
#3005 = VECTOR('',#10174,1.) ;
#3006 = VECTOR('',#10177,1.) ;
#3007 = VECTOR('',#10178,1.) ;
#3008 = VECTOR('',#10187,1.) ;
#3009 = VECTOR('',#10190,1.) ;
#3010 = VECTOR('',#10195,1.) ;
#3011 = VECTOR('',#10198,1.) ;
#3012 = VECTOR('',#10203,1.) ;
#3013 = VECTOR('',#10206,1.) ;
#3014 = VECTOR('',#10209,1.) ;
#3015 = VECTOR('',#10210,1.) ;
#3016 = VECTOR('',#10211,1.) ;
#3017 = VECTOR('',#10212,1.) ;
#3018 = VECTOR('',#10213,1.) ;
#3019 = VECTOR('',#10218,1.) ;
#3020 = VECTOR('',#10221,0.17) ;
#3021 = VECTOR('',#10226,1.) ;
#3022 = VECTOR('',#10229,1.) ;
#3023 = VECTOR('',#10234,1.) ;
#3024 = VECTOR('',#10237,1.) ;
#3025 = VECTOR('',#10242,1.) ;
#3026 = VECTOR('',#10243,1.) ;
#3027 = VECTOR('',#10248,1.) ;
#3028 = VECTOR('',#10249,1.) ;
#3029 = VECTOR('',#10250,1.) ;
#3030 = VECTOR('',#10251,1.) ;
#3031 = VECTOR('',#10254,1.) ;
#3032 = VECTOR('',#10257,1.) ;
#3033 = VECTOR('',#10258,1.) ;
#3034 = VECTOR('',#10261,0.17) ;
#3035 = VECTOR('',#10268,0.31) ;
#3036 = VECTOR('',#10271,1.) ;
#3037 = VECTOR('',#10272,1.) ;
#3038 = VECTOR('',#10275,1.) ;
#3039 = VECTOR('',#10290,0.26) ;
#3040 = VECTOR('',#10297,1.) ;
#3041 = VECTOR('',#10298,1.) ;
#3042 = VECTOR('',#10299,1.) ;
#3043 = VECTOR('',#10300,1.) ;
#3044 = VECTOR('',#10303,1.) ;
#3045 = VECTOR('',#10304,1.) ;
#3046 = VECTOR('',#10305,1.) ;
#3047 = VECTOR('',#10308,1.) ;
#3048 = VECTOR('',#10309,1.) ;
#3049 = VECTOR('',#10312,1.) ;
#3050 = VECTOR('',#10313,1.) ;
#3051 = VECTOR('',#10316,1.) ;
#3052 = VECTOR('',#10319,1.) ;
#3053 = VECTOR('',#10320,1.) ;
#3054 = VECTOR('',#10321,1.) ;
#3055 = VECTOR('',#10322,1.) ;
#3056 = VECTOR('',#10325,1.) ;
#3057 = VECTOR('',#10326,1.) ;
#3058 = VECTOR('',#10327,1.) ;
#3059 = VECTOR('',#10330,1.) ;
#3060 = VECTOR('',#10331,1.) ;
#3061 = VECTOR('',#10334,1.) ;
#3062 = VECTOR('',#10335,1.) ;
#3063 = VECTOR('',#10338,1.) ;
#3064 = VECTOR('',#10341,1.) ;
#3065 = VECTOR('',#10342,1.) ;
#3066 = VECTOR('',#10343,1.) ;
#3067 = VECTOR('',#10344,1.) ;
#3068 = VECTOR('',#10347,1.) ;
#3069 = VECTOR('',#10348,1.) ;
#3070 = VECTOR('',#10349,1.) ;
#3071 = VECTOR('',#10352,1.) ;
#3072 = VECTOR('',#10353,1.) ;
#3073 = VECTOR('',#10356,1.) ;
#3074 = VECTOR('',#10357,1.) ;
#3075 = VECTOR('',#10360,1.) ;
#3076 = VECTOR('',#10365,0.69) ;
#3077 = VECTOR('',#10372,0.81) ;
#3078 = VECTOR('',#10385,1.09) ;
#3079 = VECTOR('',#10390,1.21) ;
#3080 = VECTOR('',#10403,1.3) ;
#3081 = VECTOR('',#10414,1.1) ;
#3082 = VECTOR('',#10421,1.2) ;
#3083 = VECTOR('',#10434,0.7) ;
#3084 = VECTOR('',#10441,0.8) ;
#3085 = VECTOR('',#10460,0.25) ;
#3086 = VECTOR('',#10479,0.13) ;
#3087 = VECTOR('',#10486,0.7) ;
#3088 = VECTOR('',#10495,0.8) ;
#3089 = VECTOR('',#10508,0.2) ;
#3090 = VECTOR('',#10517,0.69) ;
#3091 = VECTOR('',#10530,0.12) ;
#3092 = VECTOR('',#10541,1.) ;
#3093 = VECTOR('',#10542,1.) ;
#3094 = VECTOR('',#10543,1.) ;
#3095 = VECTOR('',#10544,1.) ;
#3096 = VECTOR('',#10549,1.) ;
#3097 = VECTOR('',#10550,1.) ;
#3098 = VECTOR('',#10553,1.) ;
#3099 = VECTOR('',#10554,1.) ;
#3100 = VECTOR('',#10555,1.) ;
#3101 = VECTOR('',#10560,1.) ;
#3102 = VECTOR('',#10565,1.) ;
#3103 = VECTOR('',#10570,1.) ;
#3104 = VECTOR('',#10573,1.) ;
#3105 = VECTOR('',#10576,1.) ;
#3106 = VECTOR('',#10581,0.13) ;
#3107 = VECTOR('',#10592,1.) ;
#3108 = VECTOR('',#10595,0.41) ;
#3109 = VECTOR('',#10600,1.) ;
#3110 = VECTOR('',#10605,0.81) ;
#3111 = VECTOR('',#10618,1.2) ;
#3112 = VECTOR('',#10657,0.4) ;
#3113 = VECTOR('',#10672,0.4) ;
#3114 = VECTOR('',#10681,0.3) ;
#3115 = VECTOR('',#10686,0.3) ;
#3116 = VECTOR('',#10703,0.4) ;
#3117 = VECTOR('',#10710,0.45) ;
#3118 = VECTOR('',#10723,0.13) ;
#3119 = VECTOR('',#10730,0.71) ;
#3120 = VECTOR('',#10739,0.85) ;
#3121 = VECTOR('',#10752,0.7) ;
#3122 = VECTOR('',#10765,0.12) ;
#3123 = VECTOR('',#10798,0.13) ;
#3124 = VECTOR('',#10803,1.) ;
#3125 = VECTOR('',#10804,1.) ;
#3126 = VECTOR('',#10805,1.) ;
#3127 = VECTOR('',#10806,1.) ;
#3128 = VECTOR('',#10809,1.) ;
#3129 = VECTOR('',#10810,1.) ;
#3130 = VECTOR('',#10811,1.) ;
#3131 = VECTOR('',#10814,1.) ;
#3132 = VECTOR('',#10815,1.) ;
#3133 = VECTOR('',#10816,1.) ;
#3134 = VECTOR('',#10819,1.) ;
#3135 = VECTOR('',#10822,1.) ;
#3136 = VECTOR('',#10823,1.) ;
#3137 = VECTOR('',#10824,1.) ;
#3138 = VECTOR('',#10827,1.) ;
#3139 = VECTOR('',#10832,1.) ;
#3140 = VECTOR('',#10833,1.) ;
#3141 = VECTOR('',#10836,0.13) ;
#3142 = VECTOR('',#10843,1.) ;
#3143 = VECTOR('',#10846,1.) ;
#3144 = VECTOR('',#10847,1.) ;
#3145 = VECTOR('',#10852,1.) ;
#3146 = VECTOR('',#10853,1.) ;
#3147 = VECTOR('',#10856,1.) ;
#3148 = VECTOR('',#10859,1.) ;
#3149 = VECTOR('',#10860,1.) ;
#3150 = VECTOR('',#10863,1.) ;
#3151 = VECTOR('',#10876,0.2) ;
#3152 = VECTOR('',#10885,0.125) ;
#3153 = VECTOR('',#11208,0.025) ;
#3154 = VECTOR('',#11219,0.025) ;
#3155 = VECTOR('',#11226,0.025) ;
#3156 = VECTOR('',#11231,0.025) ;
#3157 = VECTOR('',#11236,0.025) ;
#3158 = VECTOR('',#11241,0.025) ;
#3159 = VECTOR('',#11248,0.025) ;
#3160 = VECTOR('',#11257,0.025) ;
#3161 = VECTOR('',#11264,0.025) ;
#3162 = VECTOR('',#11273,0.025) ;
#3163 = VECTOR('',#11280,0.025) ;
#3164 = VECTOR('',#11285,0.025) ;
#3165 = VECTOR('',#11290,0.025) ;
#3166 = VECTOR('',#11295,0.025) ;
#3167 = VECTOR('',#11302,0.025) ;
#3168 = VECTOR('',#11311,0.025) ;
#3169 = VECTOR('',#11318,0.025) ;
#3170 = VECTOR('',#11327,0.025) ;
#3171 = VECTOR('',#11334,0.025) ;
#3172 = VECTOR('',#11339,0.025) ;
#3173 = VECTOR('',#11344,0.025) ;
#3174 = VECTOR('',#11349,0.025) ;
#3175 = VECTOR('',#11356,0.025) ;
#3176 = VECTOR('',#11365,0.025) ;
#3177 = VECTOR('',#11372,0.025) ;
#3178 = VECTOR('',#11381,0.025) ;
#3179 = VECTOR('',#11388,0.025) ;
#3180 = VECTOR('',#11393,0.025) ;
#3181 = VECTOR('',#11398,0.025) ;
#3182 = VECTOR('',#11403,0.025) ;
#3183 = VECTOR('',#11410,0.025) ;
#3184 = VECTOR('',#11419,0.025) ;
#3185 = VECTOR('',#11426,0.025) ;
#3186 = VECTOR('',#11435,0.025) ;
#3187 = VECTOR('',#11442,0.025) ;
#3188 = VECTOR('',#11447,0.025) ;
#3189 = VECTOR('',#11452,0.025) ;
#3190 = VECTOR('',#11457,0.025) ;
#3191 = VECTOR('',#11464,0.025) ;
#3192 = VECTOR('',#11473,0.025) ;
#3193 = VECTOR('',#11494,0.35) ;
#3194 = VECTOR('',#11499,0.2) ;
#3195 = VECTOR('',#11502,0.2) ;
#3196 = VECTOR('',#11513,1.) ;
#3197 = VECTOR('',#11514,1.) ;
#3198 = VECTOR('',#11515,1.) ;
#3199 = VECTOR('',#11516,1.) ;
#3200 = VECTOR('',#11519,1.) ;
#3201 = VECTOR('',#11520,1.) ;
#3202 = VECTOR('',#11521,1.) ;
#3203 = VECTOR('',#11524,1.) ;
#3204 = VECTOR('',#11525,1.) ;
#3205 = VECTOR('',#11528,1.) ;
#3206 = VECTOR('',#11529,1.) ;
#3207 = VECTOR('',#11532,1.) ;
#3208 = VECTOR('',#11537,0.21) ;
#3209 = VECTOR('',#11544,1.) ;
#3210 = VECTOR('',#11545,1.) ;
#3211 = VECTOR('',#11546,1.) ;
#3212 = VECTOR('',#11547,1.) ;
#3213 = VECTOR('',#11550,1.) ;
#3214 = VECTOR('',#11551,1.) ;
#3215 = VECTOR('',#11552,1.) ;
#3216 = VECTOR('',#11553,1.) ;
#3217 = VECTOR('',#11556,1.) ;
#3218 = VECTOR('',#11557,1.) ;
#3219 = VECTOR('',#11560,1.) ;
#3220 = VECTOR('',#11563,1.) ;
#3221 = VECTOR('',#11758,0.025) ;
#3222 = VECTOR('',#11769,0.025) ;
#3223 = VECTOR('',#11776,0.025) ;
#3224 = VECTOR('',#11781,0.025) ;
#3225 = VECTOR('',#11786,0.025) ;
#3226 = VECTOR('',#11791,0.025) ;
#3227 = VECTOR('',#11798,0.025) ;
#3228 = VECTOR('',#11807,0.025) ;
#3229 = VECTOR('',#11814,0.025) ;
#3230 = VECTOR('',#11823,0.025) ;
#3231 = VECTOR('',#11830,0.025) ;
#3232 = VECTOR('',#11835,0.025) ;
#3233 = VECTOR('',#11840,0.025) ;
#3234 = VECTOR('',#11845,0.025) ;
#3235 = VECTOR('',#11852,0.025) ;
#3236 = VECTOR('',#11861,0.025) ;
#3237 = VECTOR('',#11868,0.025) ;
#3238 = VECTOR('',#11877,0.025) ;
#3239 = VECTOR('',#11884,0.025) ;
#3240 = VECTOR('',#11889,0.025) ;
#3241 = VECTOR('',#11894,0.025) ;
#3242 = VECTOR('',#11899,0.025) ;
#3243 = VECTOR('',#11906,0.025) ;
#3244 = VECTOR('',#11915,0.025) ;
#3245 = VECTOR('',#11926,0.15) ;
#3246 = VECTOR('',#11933,1.) ;
#3247 = VECTOR('',#11934,1.) ;
#3248 = VECTOR('',#11935,1.) ;
#3249 = VECTOR('',#11936,1.) ;
#3250 = VECTOR('',#11939,1.) ;
#3251 = VECTOR('',#11940,1.) ;
#3252 = VECTOR('',#11941,1.) ;
#3253 = VECTOR('',#11942,1.) ;
#3254 = VECTOR('',#11945,1.) ;
#3255 = VECTOR('',#11946,1.) ;
#3256 = VECTOR('',#11949,1.) ;
#3257 = VECTOR('',#11952,1.) ;
#3258 = VECTOR('',#11961,0.15) ;
#3259 = VECTOR('',#11972,0.15) ;
#3260 = VECTOR('',#11985,0.15) ;
#3261 = VECTOR('',#11998,0.15) ;
#3262 = VECTOR('',#12261,0.02) ;
#3263 = VECTOR('',#12272,0.02) ;
#3264 = VECTOR('',#12279,0.02) ;
#3265 = VECTOR('',#12284,0.02) ;
#3266 = VECTOR('',#12289,0.02) ;
#3267 = VECTOR('',#12294,0.02) ;
#3268 = VECTOR('',#12301,0.02) ;
#3269 = VECTOR('',#12310,0.02) ;
#3270 = VECTOR('',#12317,0.02) ;
#3271 = VECTOR('',#12326,0.02) ;
#3272 = VECTOR('',#12333,0.02) ;
#3273 = VECTOR('',#12338,0.02) ;
#3274 = VECTOR('',#12343,0.02) ;
#3275 = VECTOR('',#12348,0.02) ;
#3276 = VECTOR('',#12355,0.02) ;
#3277 = VECTOR('',#12364,0.02) ;
#3278 = VECTOR('',#12371,0.02) ;
#3279 = VECTOR('',#12380,0.02) ;
#3280 = VECTOR('',#12387,0.02) ;
#3281 = VECTOR('',#12392,0.02) ;
#3282 = VECTOR('',#12397,0.02) ;
#3283 = VECTOR('',#12402,0.02) ;
#3284 = VECTOR('',#12409,0.02) ;
#3285 = VECTOR('',#12418,0.02) ;
#3286 = VECTOR('',#12425,0.02) ;
#3287 = VECTOR('',#12434,0.02) ;
#3288 = VECTOR('',#12441,0.02) ;
#3289 = VECTOR('',#12446,0.02) ;
#3290 = VECTOR('',#12451,0.02) ;
#3291 = VECTOR('',#12456,0.02) ;
#3292 = VECTOR('',#12463,0.02) ;
#3293 = VECTOR('',#12472,0.02) ;
#3294 = VECTOR('',#12507,0.08) ;
#3295 = VECTOR('',#12512,1.) ;
#3296 = VECTOR('',#12513,1.) ;
#3297 = VECTOR('',#12514,1.) ;
#3298 = VECTOR('',#12515,1.) ;
#3299 = VECTOR('',#12518,1.) ;
#3300 = VECTOR('',#12519,1.) ;
#3301 = VECTOR('',#12520,1.) ;
#3302 = VECTOR('',#12523,1.) ;
#3303 = VECTOR('',#12524,1.) ;
#3304 = VECTOR('',#12525,1.) ;
#3305 = VECTOR('',#12528,1.) ;
#3306 = VECTOR('',#12529,1.) ;
#3307 = VECTOR('',#12530,1.) ;
#3308 = VECTOR('',#12531,1.) ;
#3309 = VECTOR('',#12534,1.) ;
#3310 = VECTOR('',#12535,1.) ;
#3311 = VECTOR('',#12536,1.) ;
#3312 = VECTOR('',#12539,1.) ;
#3313 = VECTOR('',#12540,1.) ;
#3314 = VECTOR('',#12541,1.) ;
#3315 = VECTOR('',#12544,1.) ;
#3316 = VECTOR('',#12545,1.) ;
#3317 = VECTOR('',#12548,1.) ;
#3318 = VECTOR('',#12551,1.) ;
#3319 = VECTOR('',#12558,1.) ;
#3320 = VECTOR('',#12559,1.) ;
#3321 = VECTOR('',#12560,1.) ;
#3322 = VECTOR('',#12561,1.) ;
#3323 = VECTOR('',#12564,1.) ;
#3324 = VECTOR('',#12565,1.) ;
#3325 = VECTOR('',#12566,1.) ;
#3326 = VECTOR('',#12569,1.) ;
#3327 = VECTOR('',#12570,1.) ;
#3328 = VECTOR('',#12571,1.) ;
#3329 = VECTOR('',#12574,1.) ;
#3330 = VECTOR('',#12575,1.) ;
#3331 = VECTOR('',#12582,0.16) ;
#3332 = VECTOR('',#12587,1.) ;
#3333 = VECTOR('',#12588,1.) ;
#3334 = VECTOR('',#12589,1.) ;
#3335 = VECTOR('',#12590,1.) ;
#3336 = VECTOR('',#12593,1.) ;
#3337 = VECTOR('',#12594,1.) ;
#3338 = VECTOR('',#12595,1.) ;
#3339 = VECTOR('',#12596,1.) ;
#3340 = VECTOR('',#12599,1.) ;
#3341 = VECTOR('',#12600,1.) ;
#3342 = VECTOR('',#12603,1.) ;
#3343 = VECTOR('',#12606,1.) ;
#3344 = VECTOR('',#12625,0.15) ;
#3345 = VECTOR('',#12632,0.025) ;
#3346 = VECTOR('',#12643,0.025) ;
#3347 = VECTOR('',#12656,0.115) ;
#3348 = VECTOR('',#12667,0.025) ;
#3349 = VECTOR('',#12678,0.025) ;
#3350 = VECTOR('',#12691,1.) ;
#3351 = VECTOR('',#12692,1.) ;
#3352 = VECTOR('',#12693,1.) ;
#3353 = VECTOR('',#12694,1.) ;
#3354 = VECTOR('',#12695,1.) ;
#3355 = VECTOR('',#12700,1.) ;
#3356 = VECTOR('',#12701,1.) ;
#3357 = VECTOR('',#12702,1.) ;
#3358 = VECTOR('',#12705,1.) ;
#3359 = VECTOR('',#12706,1.) ;
#3360 = VECTOR('',#12707,1.) ;
#3361 = VECTOR('',#12712,1.) ;
#3362 = VECTOR('',#12713,1.) ;
#3363 = VECTOR('',#12714,1.) ;
#3364 = VECTOR('',#12719,1.) ;
#3365 = VECTOR('',#12720,1.) ;
#3366 = VECTOR('',#12721,1.) ;
#3367 = VECTOR('',#12722,1.) ;
#3368 = VECTOR('',#12723,1.) ;
#3369 = VECTOR('',#12726,1.) ;
#3370 = VECTOR('',#12727,1.) ;
#3371 = VECTOR('',#12730,1.) ;
#3372 = VECTOR('',#12731,1.) ;
#3373 = VECTOR('',#12736,0.21) ;
#3374 = VECTOR('',#12737,0.21) ;
#3375 = VECTOR('',#12742,1.) ;
#3376 = VECTOR('',#12743,1.) ;
#3377 = VECTOR('',#12744,1.) ;
#3378 = VECTOR('',#12747,1.) ;
#3379 = VECTOR('',#12748,1.) ;
#3380 = VECTOR('',#12759,0.2) ;
#3381 = VECTOR('',#12770,0.04) ;
#3382 = VECTOR('',#12781,0.04) ;
#3383 = VECTOR('',#12794,0.29) ;
#3384 = VECTOR('',#12827,0.15) ;
#3385 = VECTOR('',#12836,0.275) ;
#3386 = VECTOR('',#12849,0.15) ;
#3387 = VECTOR('',#12858,0.275) ;
#3388 = VERTEX_POINT('',#12889) ;
#3389 = VERTEX_POINT('',#12890) ;
#3390 = VERTEX_POINT('',#12892) ;
#3391 = VERTEX_POINT('',#12894) ;
#3392 = VERTEX_POINT('',#12898) ;
#3393 = VERTEX_POINT('',#12900) ;
#3394 = VERTEX_POINT('',#12902) ;
#3395 = VERTEX_POINT('',#12904) ;
#3396 = VERTEX_POINT('',#12908) ;
#3397 = VERTEX_POINT('',#12910) ;
#3398 = VERTEX_POINT('',#12912) ;
#3399 = VERTEX_POINT('',#12916) ;
#3400 = VERTEX_POINT('',#12922) ;
#3401 = VERTEX_POINT('',#12925) ;
#3402 = VERTEX_POINT('',#12927) ;
#3403 = VERTEX_POINT('',#12929) ;
#3404 = VERTEX_POINT('',#12930) ;
#3405 = VERTEX_POINT('',#12932) ;
#3406 = VERTEX_POINT('',#12934) ;
#3407 = VERTEX_POINT('',#12937) ;
#3408 = VERTEX_POINT('',#12938) ;
#3409 = VERTEX_POINT('',#12940) ;
#3410 = VERTEX_POINT('',#12942) ;
#3411 = VERTEX_POINT('',#12945) ;
#3412 = VERTEX_POINT('',#12947) ;
#3413 = VERTEX_POINT('',#12950) ;
#3414 = VERTEX_POINT('',#12952) ;
#3415 = VERTEX_POINT('',#12957) ;
#3416 = VERTEX_POINT('',#12959) ;
#3417 = VERTEX_POINT('',#12964) ;
#3418 = VERTEX_POINT('',#12966) ;
#3419 = VERTEX_POINT('',#12970) ;
#3420 = VERTEX_POINT('',#12971) ;
#3421 = VERTEX_POINT('',#12973) ;
#3422 = VERTEX_POINT('',#12975) ;
#3423 = VERTEX_POINT('',#12979) ;
#3424 = VERTEX_POINT('',#12981) ;
#3425 = VERTEX_POINT('',#12985) ;
#3426 = VERTEX_POINT('',#12989) ;
#3427 = VERTEX_POINT('',#12993) ;
#3428 = VERTEX_POINT('',#12995) ;
#3429 = VERTEX_POINT('',#12997) ;
#3430 = VERTEX_POINT('',#12999) ;
#3431 = VERTEX_POINT('',#13003) ;
#3432 = VERTEX_POINT('',#13005) ;
#3433 = VERTEX_POINT('',#13009) ;
#3434 = VERTEX_POINT('',#13010) ;
#3435 = VERTEX_POINT('',#13012) ;
#3436 = VERTEX_POINT('',#13014) ;
#3437 = VERTEX_POINT('',#13018) ;
#3438 = VERTEX_POINT('',#13020) ;
#3439 = VERTEX_POINT('',#13024) ;
#3440 = VERTEX_POINT('',#13028) ;
#3441 = VERTEX_POINT('',#13032) ;
#3442 = VERTEX_POINT('',#13034) ;
#3443 = VERTEX_POINT('',#13036) ;
#3444 = VERTEX_POINT('',#13038) ;
#3445 = VERTEX_POINT('',#13042) ;
#3446 = VERTEX_POINT('',#13044) ;
#3447 = VERTEX_POINT('',#13048) ;
#3448 = VERTEX_POINT('',#13054) ;
#3449 = VERTEX_POINT('',#13056) ;
#3450 = VERTEX_POINT('',#13060) ;
#3451 = VERTEX_POINT('',#13065) ;
#3452 = VERTEX_POINT('',#13067) ;
#3453 = VERTEX_POINT('',#13071) ;
#3454 = VERTEX_POINT('',#13077) ;
#3455 = VERTEX_POINT('',#13079) ;
#3456 = VERTEX_POINT('',#13083) ;
#3457 = VERTEX_POINT('',#13085) ;
#3458 = VERTEX_POINT('',#13089) ;
#3459 = VERTEX_POINT('',#13090) ;
#3460 = VERTEX_POINT('',#13092) ;
#3461 = VERTEX_POINT('',#13094) ;
#3462 = VERTEX_POINT('',#13106) ;
#3463 = VERTEX_POINT('',#13107) ;
#3464 = VERTEX_POINT('',#13109) ;
#3465 = VERTEX_POINT('',#13111) ;
#3466 = VERTEX_POINT('',#13123) ;
#3467 = VERTEX_POINT('',#13127) ;
#3468 = VERTEX_POINT('',#13143) ;
#3469 = VERTEX_POINT('',#13144) ;
#3470 = VERTEX_POINT('',#13146) ;
#3471 = VERTEX_POINT('',#13148) ;
#3472 = VERTEX_POINT('',#13152) ;
#3473 = VERTEX_POINT('',#13154) ;
#3474 = VERTEX_POINT('',#13157) ;
#3475 = VERTEX_POINT('',#13160) ;
#3476 = VERTEX_POINT('',#13162) ;
#3477 = VERTEX_POINT('',#13166) ;
#3478 = VERTEX_POINT('',#13168) ;
#3479 = VERTEX_POINT('',#13170) ;
#3480 = VERTEX_POINT('',#13172) ;
#3481 = VERTEX_POINT('',#13175) ;
#3482 = VERTEX_POINT('',#13180) ;
#3483 = VERTEX_POINT('',#13184) ;
#3484 = VERTEX_POINT('',#13185) ;
#3485 = VERTEX_POINT('',#13187) ;
#3486 = VERTEX_POINT('',#13189) ;
#3487 = VERTEX_POINT('',#13193) ;
#3488 = VERTEX_POINT('',#13194) ;
#3489 = VERTEX_POINT('',#13196) ;
#3490 = VERTEX_POINT('',#13198) ;
#3491 = VERTEX_POINT('',#13204) ;
#3492 = VERTEX_POINT('',#13208) ;
#3493 = VERTEX_POINT('',#13210) ;
#3494 = VERTEX_POINT('',#13216) ;
#3495 = VERTEX_POINT('',#13220) ;
#3496 = VERTEX_POINT('',#13224) ;
#3497 = VERTEX_POINT('',#13228) ;
#3498 = VERTEX_POINT('',#13239) ;
#3499 = VERTEX_POINT('',#13241) ;
#3500 = VERTEX_POINT('',#13246) ;
#3501 = VERTEX_POINT('',#13247) ;
#3502 = VERTEX_POINT('',#13249) ;
#3503 = VERTEX_POINT('',#13251) ;
#3504 = VERTEX_POINT('',#13255) ;
#3505 = VERTEX_POINT('',#13257) ;
#3506 = VERTEX_POINT('',#13261) ;
#3507 = VERTEX_POINT('',#13265) ;
#3508 = VERTEX_POINT('',#13271) ;
#3509 = VERTEX_POINT('',#13272) ;
#3510 = VERTEX_POINT('',#13274) ;
#3511 = VERTEX_POINT('',#13276) ;
#3512 = VERTEX_POINT('',#13280) ;
#3513 = VERTEX_POINT('',#13282) ;
#3514 = VERTEX_POINT('',#13286) ;
#3515 = VERTEX_POINT('',#13290) ;
#3516 = VERTEX_POINT('',#13296) ;
#3517 = VERTEX_POINT('',#13297) ;
#3518 = VERTEX_POINT('',#13299) ;
#3519 = VERTEX_POINT('',#13301) ;
#3520 = VERTEX_POINT('',#13305) ;
#3521 = VERTEX_POINT('',#13307) ;
#3522 = VERTEX_POINT('',#13311) ;
#3523 = VERTEX_POINT('',#13315) ;
#3524 = VERTEX_POINT('',#13321) ;
#3525 = VERTEX_POINT('',#13323) ;
#3526 = VERTEX_POINT('',#13327) ;
#3527 = VERTEX_POINT('',#13329) ;
#3528 = VERTEX_POINT('',#13334) ;
#3529 = VERTEX_POINT('',#13337) ;
#3530 = VERTEX_POINT('',#13341) ;
#3531 = VERTEX_POINT('',#13343) ;
#3532 = VERTEX_POINT('',#13348) ;
#3533 = VERTEX_POINT('',#13351) ;
#3534 = VERTEX_POINT('',#13358) ;
#3535 = VERTEX_POINT('',#13360) ;
#3536 = VERTEX_POINT('',#13364) ;
#3537 = VERTEX_POINT('',#13366) ;
#3538 = VERTEX_POINT('',#13373) ;
#3539 = VERTEX_POINT('',#13375) ;
#3540 = VERTEX_POINT('',#13379) ;
#3541 = VERTEX_POINT('',#13381) ;
#3542 = VERTEX_POINT('',#13388) ;
#3543 = VERTEX_POINT('',#13390) ;
#3544 = VERTEX_POINT('',#13393) ;
#3545 = VERTEX_POINT('',#13404) ;
#3546 = VERTEX_POINT('',#13406) ;
#3547 = VERTEX_POINT('',#13410) ;
#3548 = VERTEX_POINT('',#13412) ;
#3549 = VERTEX_POINT('',#13416) ;
#3550 = VERTEX_POINT('',#13419) ;
#3551 = VERTEX_POINT('',#13426) ;
#3552 = VERTEX_POINT('',#13428) ;
#3553 = VERTEX_POINT('',#13433) ;
#3554 = VERTEX_POINT('',#13435) ;
#3555 = VERTEX_POINT('',#13442) ;
#3556 = VERTEX_POINT('',#13444) ;
#3557 = VERTEX_POINT('',#13451) ;
#3558 = VERTEX_POINT('',#13452) ;
#3559 = VERTEX_POINT('',#13454) ;
#3560 = VERTEX_POINT('',#13456) ;
#3561 = VERTEX_POINT('',#13460) ;
#3562 = VERTEX_POINT('',#13461) ;
#3563 = VERTEX_POINT('',#13463) ;
#3564 = VERTEX_POINT('',#13467) ;
#3565 = VERTEX_POINT('',#13469) ;
#3566 = VERTEX_POINT('',#13473) ;
#3567 = VERTEX_POINT('',#13477) ;
#3568 = VERTEX_POINT('',#13481) ;
#3569 = VERTEX_POINT('',#13489) ;
#3570 = VERTEX_POINT('',#13491) ;
#3571 = VERTEX_POINT('',#13495) ;
#3572 = VERTEX_POINT('',#13496) ;
#3573 = VERTEX_POINT('',#13500) ;
#3574 = VERTEX_POINT('',#13502) ;
#3575 = VERTEX_POINT('',#13504) ;
#3576 = VERTEX_POINT('',#13507) ;
#3577 = VERTEX_POINT('',#13511) ;
#3578 = VERTEX_POINT('',#13513) ;
#3579 = VERTEX_POINT('',#13519) ;
#3580 = VERTEX_POINT('',#13522) ;
#3581 = VERTEX_POINT('',#13528) ;
#3582 = VERTEX_POINT('',#13529) ;
#3583 = VERTEX_POINT('',#13532) ;
#3584 = VERTEX_POINT('',#13533) ;
#3585 = VERTEX_POINT('',#13540) ;
#3586 = VERTEX_POINT('',#13542) ;
#3587 = VERTEX_POINT('',#13545) ;
#3588 = VERTEX_POINT('',#13546) ;
#3589 = VERTEX_POINT('',#13571) ;
#3590 = VERTEX_POINT('',#13572) ;
#3591 = VERTEX_POINT('',#13574) ;
#3592 = VERTEX_POINT('',#13579) ;
#3593 = VERTEX_POINT('',#13581) ;
#3594 = VERTEX_POINT('',#13584) ;
#3595 = VERTEX_POINT('',#13585) ;
#3596 = VERTEX_POINT('',#13610) ;
#3597 = VERTEX_POINT('',#13615) ;
#3598 = VERTEX_POINT('',#13620) ;
#3599 = VERTEX_POINT('',#13629) ;
#3600 = VERTEX_POINT('',#13631) ;
#3601 = VERTEX_POINT('',#13635) ;
#3602 = VERTEX_POINT('',#13637) ;
#3603 = VERTEX_POINT('',#13644) ;
#3604 = VERTEX_POINT('',#13646) ;
#3605 = VERTEX_POINT('',#13650) ;
#3606 = VERTEX_POINT('',#13652) ;
#3607 = VERTEX_POINT('',#13656) ;
#3608 = VERTEX_POINT('',#13659) ;
#3609 = VERTEX_POINT('',#13666) ;
#3610 = VERTEX_POINT('',#13668) ;
#3611 = VERTEX_POINT('',#13675) ;
#3612 = VERTEX_POINT('',#13677) ;
#3613 = VERTEX_POINT('',#13694) ;
#3614 = VERTEX_POINT('',#13696) ;
#3615 = VERTEX_POINT('',#13700) ;
#3616 = VERTEX_POINT('',#13701) ;
#3617 = VERTEX_POINT('',#13703) ;
#3618 = VERTEX_POINT('',#13705) ;
#3619 = VERTEX_POINT('',#13709) ;
#3620 = VERTEX_POINT('',#13711) ;
#3621 = VERTEX_POINT('',#13715) ;
#3622 = VERTEX_POINT('',#13716) ;
#3623 = VERTEX_POINT('',#13721) ;
#3624 = VERTEX_POINT('',#13723) ;
#3625 = VERTEX_POINT('',#13725) ;
#3626 = VERTEX_POINT('',#13727) ;
#3627 = VERTEX_POINT('',#13729) ;
#3628 = VERTEX_POINT('',#13731) ;
#3629 = VERTEX_POINT('',#13734) ;
#3630 = VERTEX_POINT('',#13737) ;
#3631 = VERTEX_POINT('',#13741) ;
#3632 = VERTEX_POINT('',#13745) ;
#3633 = VERTEX_POINT('',#13749) ;
#3634 = VERTEX_POINT('',#13751) ;
#3635 = VERTEX_POINT('',#13755) ;
#3636 = VERTEX_POINT('',#13761) ;
#3637 = VERTEX_POINT('',#13769) ;
#3638 = VERTEX_POINT('',#13771) ;
#3639 = VERTEX_POINT('',#13774) ;
#3640 = VERTEX_POINT('',#13779) ;
#3641 = VERTEX_POINT('',#13785) ;
#3642 = VERTEX_POINT('',#13786) ;
#3643 = VERTEX_POINT('',#13790) ;
#3644 = VERTEX_POINT('',#13791) ;
#3645 = VERTEX_POINT('',#13793) ;
#3646 = VERTEX_POINT('',#13797) ;
#3647 = VERTEX_POINT('',#13798) ;
#3648 = VERTEX_POINT('',#13800) ;
#3649 = VERTEX_POINT('',#13802) ;
#3650 = VERTEX_POINT('',#13806) ;
#3651 = VERTEX_POINT('',#13807) ;
#3652 = VERTEX_POINT('',#13809) ;
#3653 = VERTEX_POINT('',#13811) ;
#3654 = VERTEX_POINT('',#13815) ;
#3655 = VERTEX_POINT('',#13816) ;
#3656 = VERTEX_POINT('',#13818) ;
#3657 = VERTEX_POINT('',#13820) ;
#3658 = VERTEX_POINT('',#13824) ;
#3659 = VERTEX_POINT('',#13825) ;
#3660 = VERTEX_POINT('',#13827) ;
#3661 = VERTEX_POINT('',#13831) ;
#3662 = VERTEX_POINT('',#13832) ;
#3663 = VERTEX_POINT('',#13836) ;
#3664 = VERTEX_POINT('',#13837) ;
#3665 = VERTEX_POINT('',#13841) ;
#3666 = VERTEX_POINT('',#13842) ;
#3667 = VERTEX_POINT('',#13846) ;
#3668 = VERTEX_POINT('',#13847) ;
#3669 = VERTEX_POINT('',#13849) ;
#3670 = VERTEX_POINT('',#13853) ;
#3671 = VERTEX_POINT('',#13854) ;
#3672 = VERTEX_POINT('',#13856) ;
#3673 = VERTEX_POINT('',#13858) ;
#3674 = VERTEX_POINT('',#13862) ;
#3675 = VERTEX_POINT('',#13863) ;
#3676 = VERTEX_POINT('',#13865) ;
#3677 = VERTEX_POINT('',#13867) ;
#3678 = VERTEX_POINT('',#13871) ;
#3679 = VERTEX_POINT('',#13872) ;
#3680 = VERTEX_POINT('',#13874) ;
#3681 = VERTEX_POINT('',#13876) ;
#3682 = VERTEX_POINT('',#13880) ;
#3683 = VERTEX_POINT('',#13881) ;
#3684 = VERTEX_POINT('',#13883) ;
#3685 = VERTEX_POINT('',#13887) ;
#3686 = VERTEX_POINT('',#13888) ;
#3687 = VERTEX_POINT('',#13892) ;
#3688 = VERTEX_POINT('',#13893) ;
#3689 = VERTEX_POINT('',#13897) ;
#3690 = VERTEX_POINT('',#13898) ;
#3691 = VERTEX_POINT('',#13902) ;
#3692 = VERTEX_POINT('',#13903) ;
#3693 = VERTEX_POINT('',#13905) ;
#3694 = VERTEX_POINT('',#13909) ;
#3695 = VERTEX_POINT('',#13910) ;
#3696 = VERTEX_POINT('',#13912) ;
#3697 = VERTEX_POINT('',#13914) ;
#3698 = VERTEX_POINT('',#13918) ;
#3699 = VERTEX_POINT('',#13919) ;
#3700 = VERTEX_POINT('',#13921) ;
#3701 = VERTEX_POINT('',#13923) ;
#3702 = VERTEX_POINT('',#13927) ;
#3703 = VERTEX_POINT('',#13928) ;
#3704 = VERTEX_POINT('',#13930) ;
#3705 = VERTEX_POINT('',#13932) ;
#3706 = VERTEX_POINT('',#13936) ;
#3707 = VERTEX_POINT('',#13937) ;
#3708 = VERTEX_POINT('',#13939) ;
#3709 = VERTEX_POINT('',#13943) ;
#3710 = VERTEX_POINT('',#13944) ;
#3711 = VERTEX_POINT('',#13948) ;
#3712 = VERTEX_POINT('',#13949) ;
#3713 = VERTEX_POINT('',#13953) ;
#3714 = VERTEX_POINT('',#13954) ;
#3715 = VERTEX_POINT('',#13958) ;
#3716 = VERTEX_POINT('',#13959) ;
#3717 = VERTEX_POINT('',#13961) ;
#3718 = VERTEX_POINT('',#13965) ;
#3719 = VERTEX_POINT('',#13966) ;
#3720 = VERTEX_POINT('',#13968) ;
#3721 = VERTEX_POINT('',#13970) ;
#3722 = VERTEX_POINT('',#13974) ;
#3723 = VERTEX_POINT('',#13975) ;
#3724 = VERTEX_POINT('',#13977) ;
#3725 = VERTEX_POINT('',#13979) ;
#3726 = VERTEX_POINT('',#13983) ;
#3727 = VERTEX_POINT('',#13984) ;
#3728 = VERTEX_POINT('',#13986) ;
#3729 = VERTEX_POINT('',#13988) ;
#3730 = VERTEX_POINT('',#13992) ;
#3731 = VERTEX_POINT('',#13993) ;
#3732 = VERTEX_POINT('',#13995) ;
#3733 = VERTEX_POINT('',#13999) ;
#3734 = VERTEX_POINT('',#14000) ;
#3735 = VERTEX_POINT('',#14004) ;
#3736 = VERTEX_POINT('',#14005) ;
#3737 = VERTEX_POINT('',#14009) ;
#3738 = VERTEX_POINT('',#14010) ;
#3739 = VERTEX_POINT('',#14014) ;
#3740 = VERTEX_POINT('',#14015) ;
#3741 = VERTEX_POINT('',#14017) ;
#3742 = VERTEX_POINT('',#14021) ;
#3743 = VERTEX_POINT('',#14022) ;
#3744 = VERTEX_POINT('',#14024) ;
#3745 = VERTEX_POINT('',#14026) ;
#3746 = VERTEX_POINT('',#14030) ;
#3747 = VERTEX_POINT('',#14031) ;
#3748 = VERTEX_POINT('',#14033) ;
#3749 = VERTEX_POINT('',#14035) ;
#3750 = VERTEX_POINT('',#14039) ;
#3751 = VERTEX_POINT('',#14040) ;
#3752 = VERTEX_POINT('',#14042) ;
#3753 = VERTEX_POINT('',#14044) ;
#3754 = VERTEX_POINT('',#14048) ;
#3755 = VERTEX_POINT('',#14049) ;
#3756 = VERTEX_POINT('',#14051) ;
#3757 = VERTEX_POINT('',#14055) ;
#3758 = VERTEX_POINT('',#14056) ;
#3759 = VERTEX_POINT('',#14060) ;
#3760 = VERTEX_POINT('',#14062) ;
#3761 = VERTEX_POINT('',#14064) ;
#3762 = VERTEX_POINT('',#14070) ;
#3763 = VERTEX_POINT('',#14085) ;
#3764 = VERTEX_POINT('',#14089) ;
#3765 = VERTEX_POINT('',#14091) ;
#3766 = VERTEX_POINT('',#14096) ;
#3767 = VERTEX_POINT('',#14101) ;
#3768 = VERTEX_POINT('',#14103) ;
#3769 = VERTEX_POINT('',#14108) ;
#3770 = VERTEX_POINT('',#14123) ;
#3771 = VERTEX_POINT('',#14127) ;
#3772 = VERTEX_POINT('',#14129) ;
#3773 = VERTEX_POINT('',#14134) ;
#3774 = VERTEX_POINT('',#14139) ;
#3775 = VERTEX_POINT('',#14141) ;
#3776 = VERTEX_POINT('',#14146) ;
#3777 = VERTEX_POINT('',#14161) ;
#3778 = VERTEX_POINT('',#14165) ;
#3779 = VERTEX_POINT('',#14167) ;
#3780 = VERTEX_POINT('',#14172) ;
#3781 = VERTEX_POINT('',#14177) ;
#3782 = VERTEX_POINT('',#14179) ;
#3783 = VERTEX_POINT('',#14184) ;
#3784 = VERTEX_POINT('',#14199) ;
#3785 = VERTEX_POINT('',#14203) ;
#3786 = VERTEX_POINT('',#14205) ;
#3787 = VERTEX_POINT('',#14210) ;
#3788 = VERTEX_POINT('',#14215) ;
#3789 = VERTEX_POINT('',#14217) ;
#3790 = VERTEX_POINT('',#14222) ;
#3791 = VERTEX_POINT('',#14237) ;
#3792 = VERTEX_POINT('',#14241) ;
#3793 = VERTEX_POINT('',#14243) ;
#3794 = VERTEX_POINT('',#14248) ;
#3795 = VERTEX_POINT('',#14254) ;
#3796 = VERTEX_POINT('',#14256) ;
#3797 = VERTEX_POINT('',#14259) ;
#3798 = VERTEX_POINT('',#14261) ;
#3799 = VERTEX_POINT('',#14266) ;
#3800 = VERTEX_POINT('',#14270) ;
#3801 = VERTEX_POINT('',#14277) ;
#3802 = VERTEX_POINT('',#14278) ;
#3803 = VERTEX_POINT('',#14280) ;
#3804 = VERTEX_POINT('',#14282) ;
#3805 = VERTEX_POINT('',#14286) ;
#3806 = VERTEX_POINT('',#14288) ;
#3807 = VERTEX_POINT('',#14292) ;
#3808 = VERTEX_POINT('',#14296) ;
#3809 = VERTEX_POINT('',#14302) ;
#3810 = VERTEX_POINT('',#14304) ;
#3811 = VERTEX_POINT('',#14309) ;
#3812 = VERTEX_POINT('',#14310) ;
#3813 = VERTEX_POINT('',#14312) ;
#3814 = VERTEX_POINT('',#14314) ;
#3815 = VERTEX_POINT('',#14318) ;
#3816 = VERTEX_POINT('',#14319) ;
#3817 = VERTEX_POINT('',#14321) ;
#3818 = VERTEX_POINT('',#14323) ;
#3819 = VERTEX_POINT('',#14336) ;
#3820 = VERTEX_POINT('',#14337) ;
#3821 = VERTEX_POINT('',#14341) ;
#3822 = VERTEX_POINT('',#14342) ;
#3823 = VERTEX_POINT('',#14344) ;
#3824 = VERTEX_POINT('',#14348) ;
#3825 = VERTEX_POINT('',#14349) ;
#3826 = VERTEX_POINT('',#14351) ;
#3827 = VERTEX_POINT('',#14353) ;
#3828 = VERTEX_POINT('',#14357) ;
#3829 = VERTEX_POINT('',#14358) ;
#3830 = VERTEX_POINT('',#14360) ;
#3831 = VERTEX_POINT('',#14362) ;
#3832 = VERTEX_POINT('',#14366) ;
#3833 = VERTEX_POINT('',#14367) ;
#3834 = VERTEX_POINT('',#14369) ;
#3835 = VERTEX_POINT('',#14371) ;
#3836 = VERTEX_POINT('',#14375) ;
#3837 = VERTEX_POINT('',#14376) ;
#3838 = VERTEX_POINT('',#14378) ;
#3839 = VERTEX_POINT('',#14382) ;
#3840 = VERTEX_POINT('',#14383) ;
#3841 = VERTEX_POINT('',#14387) ;
#3842 = VERTEX_POINT('',#14388) ;
#3843 = VERTEX_POINT('',#14392) ;
#3844 = VERTEX_POINT('',#14393) ;
#3845 = VERTEX_POINT('',#14397) ;
#3846 = VERTEX_POINT('',#14398) ;
#3847 = VERTEX_POINT('',#14400) ;
#3848 = VERTEX_POINT('',#14404) ;
#3849 = VERTEX_POINT('',#14405) ;
#3850 = VERTEX_POINT('',#14407) ;
#3851 = VERTEX_POINT('',#14409) ;
#3852 = VERTEX_POINT('',#14413) ;
#3853 = VERTEX_POINT('',#14414) ;
#3854 = VERTEX_POINT('',#14416) ;
#3855 = VERTEX_POINT('',#14418) ;
#3856 = VERTEX_POINT('',#14422) ;
#3857 = VERTEX_POINT('',#14423) ;
#3858 = VERTEX_POINT('',#14425) ;
#3859 = VERTEX_POINT('',#14427) ;
#3860 = VERTEX_POINT('',#14431) ;
#3861 = VERTEX_POINT('',#14432) ;
#3862 = VERTEX_POINT('',#14434) ;
#3863 = VERTEX_POINT('',#14438) ;
#3864 = VERTEX_POINT('',#14439) ;
#3865 = VERTEX_POINT('',#14443) ;
#3866 = VERTEX_POINT('',#14444) ;
#3867 = VERTEX_POINT('',#14448) ;
#3868 = VERTEX_POINT('',#14449) ;
#3869 = VERTEX_POINT('',#14453) ;
#3870 = VERTEX_POINT('',#14454) ;
#3871 = VERTEX_POINT('',#14456) ;
#3872 = VERTEX_POINT('',#14460) ;
#3873 = VERTEX_POINT('',#14461) ;
#3874 = VERTEX_POINT('',#14463) ;
#3875 = VERTEX_POINT('',#14465) ;
#3876 = VERTEX_POINT('',#14469) ;
#3877 = VERTEX_POINT('',#14470) ;
#3878 = VERTEX_POINT('',#14472) ;
#3879 = VERTEX_POINT('',#14474) ;
#3880 = VERTEX_POINT('',#14478) ;
#3881 = VERTEX_POINT('',#14479) ;
#3882 = VERTEX_POINT('',#14481) ;
#3883 = VERTEX_POINT('',#14483) ;
#3884 = VERTEX_POINT('',#14487) ;
#3885 = VERTEX_POINT('',#14488) ;
#3886 = VERTEX_POINT('',#14490) ;
#3887 = VERTEX_POINT('',#14494) ;
#3888 = VERTEX_POINT('',#14495) ;
#3889 = VERTEX_POINT('',#14499) ;
#3890 = VERTEX_POINT('',#14501) ;
#3891 = VERTEX_POINT('',#14503) ;
#3892 = VERTEX_POINT('',#14509) ;
#3893 = VERTEX_POINT('',#14524) ;
#3894 = VERTEX_POINT('',#14528) ;
#3895 = VERTEX_POINT('',#14530) ;
#3896 = VERTEX_POINT('',#14535) ;
#3897 = VERTEX_POINT('',#14540) ;
#3898 = VERTEX_POINT('',#14542) ;
#3899 = VERTEX_POINT('',#14547) ;
#3900 = VERTEX_POINT('',#14562) ;
#3901 = VERTEX_POINT('',#14566) ;
#3902 = VERTEX_POINT('',#14568) ;
#3903 = VERTEX_POINT('',#14573) ;
#3904 = VERTEX_POINT('',#14578) ;
#3905 = VERTEX_POINT('',#14580) ;
#3906 = VERTEX_POINT('',#14585) ;
#3907 = VERTEX_POINT('',#14600) ;
#3908 = VERTEX_POINT('',#14604) ;
#3909 = VERTEX_POINT('',#14606) ;
#3910 = VERTEX_POINT('',#14611) ;
#3911 = VERTEX_POINT('',#14617) ;
#3912 = VERTEX_POINT('',#14619) ;
#3913 = VERTEX_POINT('',#14624) ;
#3914 = VERTEX_POINT('',#14625) ;
#3915 = VERTEX_POINT('',#14627) ;
#3916 = VERTEX_POINT('',#14629) ;
#3917 = VERTEX_POINT('',#14633) ;
#3918 = VERTEX_POINT('',#14634) ;
#3919 = VERTEX_POINT('',#14636) ;
#3920 = VERTEX_POINT('',#14638) ;
#3921 = VERTEX_POINT('',#14651) ;
#3922 = VERTEX_POINT('',#14653) ;
#3923 = VERTEX_POINT('',#14659) ;
#3924 = VERTEX_POINT('',#14661) ;
#3925 = VERTEX_POINT('',#14668) ;
#3926 = VERTEX_POINT('',#14670) ;
#3927 = VERTEX_POINT('',#14677) ;
#3928 = VERTEX_POINT('',#14679) ;
#3929 = VERTEX_POINT('',#14686) ;
#3930 = VERTEX_POINT('',#14687) ;
#3931 = VERTEX_POINT('',#14691) ;
#3932 = VERTEX_POINT('',#14692) ;
#3933 = VERTEX_POINT('',#14694) ;
#3934 = VERTEX_POINT('',#14698) ;
#3935 = VERTEX_POINT('',#14699) ;
#3936 = VERTEX_POINT('',#14701) ;
#3937 = VERTEX_POINT('',#14703) ;
#3938 = VERTEX_POINT('',#14707) ;
#3939 = VERTEX_POINT('',#14708) ;
#3940 = VERTEX_POINT('',#14710) ;
#3941 = VERTEX_POINT('',#14712) ;
#3942 = VERTEX_POINT('',#14716) ;
#3943 = VERTEX_POINT('',#14717) ;
#3944 = VERTEX_POINT('',#14719) ;
#3945 = VERTEX_POINT('',#14721) ;
#3946 = VERTEX_POINT('',#14725) ;
#3947 = VERTEX_POINT('',#14726) ;
#3948 = VERTEX_POINT('',#14728) ;
#3949 = VERTEX_POINT('',#14732) ;
#3950 = VERTEX_POINT('',#14733) ;
#3951 = VERTEX_POINT('',#14737) ;
#3952 = VERTEX_POINT('',#14738) ;
#3953 = VERTEX_POINT('',#14742) ;
#3954 = VERTEX_POINT('',#14743) ;
#3955 = VERTEX_POINT('',#14747) ;
#3956 = VERTEX_POINT('',#14748) ;
#3957 = VERTEX_POINT('',#14750) ;
#3958 = VERTEX_POINT('',#14754) ;
#3959 = VERTEX_POINT('',#14755) ;
#3960 = VERTEX_POINT('',#14757) ;
#3961 = VERTEX_POINT('',#14759) ;
#3962 = VERTEX_POINT('',#14763) ;
#3963 = VERTEX_POINT('',#14764) ;
#3964 = VERTEX_POINT('',#14766) ;
#3965 = VERTEX_POINT('',#14768) ;
#3966 = VERTEX_POINT('',#14772) ;
#3967 = VERTEX_POINT('',#14773) ;
#3968 = VERTEX_POINT('',#14775) ;
#3969 = VERTEX_POINT('',#14777) ;
#3970 = VERTEX_POINT('',#14781) ;
#3971 = VERTEX_POINT('',#14782) ;
#3972 = VERTEX_POINT('',#14784) ;
#3973 = VERTEX_POINT('',#14788) ;
#3974 = VERTEX_POINT('',#14789) ;
#3975 = VERTEX_POINT('',#14793) ;
#3976 = VERTEX_POINT('',#14794) ;
#3977 = VERTEX_POINT('',#14798) ;
#3978 = VERTEX_POINT('',#14799) ;
#3979 = VERTEX_POINT('',#14803) ;
#3980 = VERTEX_POINT('',#14804) ;
#3981 = VERTEX_POINT('',#14806) ;
#3982 = VERTEX_POINT('',#14810) ;
#3983 = VERTEX_POINT('',#14811) ;
#3984 = VERTEX_POINT('',#14813) ;
#3985 = VERTEX_POINT('',#14815) ;
#3986 = VERTEX_POINT('',#14819) ;
#3987 = VERTEX_POINT('',#14820) ;
#3988 = VERTEX_POINT('',#14822) ;
#3989 = VERTEX_POINT('',#14824) ;
#3990 = VERTEX_POINT('',#14828) ;
#3991 = VERTEX_POINT('',#14829) ;
#3992 = VERTEX_POINT('',#14831) ;
#3993 = VERTEX_POINT('',#14833) ;
#3994 = VERTEX_POINT('',#14837) ;
#3995 = VERTEX_POINT('',#14838) ;
#3996 = VERTEX_POINT('',#14840) ;
#3997 = VERTEX_POINT('',#14844) ;
#3998 = VERTEX_POINT('',#14845) ;
#3999 = VERTEX_POINT('',#14849) ;
#4000 = VERTEX_POINT('',#14850) ;
#4001 = VERTEX_POINT('',#14854) ;
#4002 = VERTEX_POINT('',#14855) ;
#4003 = VERTEX_POINT('',#14859) ;
#4004 = VERTEX_POINT('',#14860) ;
#4005 = VERTEX_POINT('',#14862) ;
#4006 = VERTEX_POINT('',#14866) ;
#4007 = VERTEX_POINT('',#14867) ;
#4008 = VERTEX_POINT('',#14869) ;
#4009 = VERTEX_POINT('',#14871) ;
#4010 = VERTEX_POINT('',#14875) ;
#4011 = VERTEX_POINT('',#14876) ;
#4012 = VERTEX_POINT('',#14878) ;
#4013 = VERTEX_POINT('',#14880) ;
#4014 = VERTEX_POINT('',#14884) ;
#4015 = VERTEX_POINT('',#14885) ;
#4016 = VERTEX_POINT('',#14887) ;
#4017 = VERTEX_POINT('',#14889) ;
#4018 = VERTEX_POINT('',#14893) ;
#4019 = VERTEX_POINT('',#14894) ;
#4020 = VERTEX_POINT('',#14896) ;
#4021 = VERTEX_POINT('',#14900) ;
#4022 = VERTEX_POINT('',#14901) ;
#4023 = VERTEX_POINT('',#14905) ;
#4024 = VERTEX_POINT('',#14907) ;
#4025 = VERTEX_POINT('',#14909) ;
#4026 = VERTEX_POINT('',#14915) ;
#4027 = VERTEX_POINT('',#14930) ;
#4028 = VERTEX_POINT('',#14934) ;
#4029 = VERTEX_POINT('',#14936) ;
#4030 = VERTEX_POINT('',#14941) ;
#4031 = VERTEX_POINT('',#14946) ;
#4032 = VERTEX_POINT('',#14948) ;
#4033 = VERTEX_POINT('',#14953) ;
#4034 = VERTEX_POINT('',#14968) ;
#4035 = VERTEX_POINT('',#14972) ;
#4036 = VERTEX_POINT('',#14974) ;
#4037 = VERTEX_POINT('',#14979) ;
#4038 = VERTEX_POINT('',#14984) ;
#4039 = VERTEX_POINT('',#14986) ;
#4040 = VERTEX_POINT('',#14991) ;
#4041 = VERTEX_POINT('',#15006) ;
#4042 = VERTEX_POINT('',#15010) ;
#4043 = VERTEX_POINT('',#15012) ;
#4044 = VERTEX_POINT('',#15017) ;
#4045 = VERTEX_POINT('',#15022) ;
#4046 = VERTEX_POINT('',#15024) ;
#4047 = VERTEX_POINT('',#15029) ;
#4048 = VERTEX_POINT('',#15044) ;
#4049 = VERTEX_POINT('',#15048) ;
#4050 = VERTEX_POINT('',#15050) ;
#4051 = VERTEX_POINT('',#15055) ;
#4052 = VERTEX_POINT('',#15073) ;
#4053 = VERTEX_POINT('',#15075) ;
#4054 = VERTEX_POINT('',#15079) ;
#4055 = VERTEX_POINT('',#15080) ;
#4056 = VERTEX_POINT('',#15082) ;
#4057 = VERTEX_POINT('',#15084) ;
#4058 = VERTEX_POINT('',#15088) ;
#4059 = VERTEX_POINT('',#15089) ;
#4060 = VERTEX_POINT('',#15094) ;
#4061 = VERTEX_POINT('',#15095) ;
#4062 = VERTEX_POINT('',#15100) ;
#4063 = VERTEX_POINT('',#15101) ;
#4064 = VERTEX_POINT('',#15103) ;
#4065 = VERTEX_POINT('',#15105) ;
#4066 = VERTEX_POINT('',#15109) ;
#4067 = VERTEX_POINT('',#15111) ;
#4068 = VERTEX_POINT('',#15115) ;
#4069 = VERTEX_POINT('',#15117) ;
#4070 = VERTEX_POINT('',#15130) ;
#4071 = VERTEX_POINT('',#15131) ;
#4072 = VERTEX_POINT('',#15133) ;
#4073 = VERTEX_POINT('',#15135) ;
#4074 = VERTEX_POINT('',#15139) ;
#4075 = VERTEX_POINT('',#15141) ;
#4076 = VERTEX_POINT('',#15145) ;
#4077 = VERTEX_POINT('',#15147) ;
#4078 = VERTEX_POINT('',#15154) ;
#4079 = VERTEX_POINT('',#15157) ;
#4080 = VERTEX_POINT('',#15161) ;
#4081 = VERTEX_POINT('',#15162) ;
#4082 = VERTEX_POINT('',#15164) ;
#4083 = VERTEX_POINT('',#15166) ;
#4084 = VERTEX_POINT('',#15170) ;
#4085 = VERTEX_POINT('',#15171) ;
#4086 = VERTEX_POINT('',#15173) ;
#4087 = VERTEX_POINT('',#15175) ;
#4088 = VERTEX_POINT('',#15188) ;
#4089 = VERTEX_POINT('',#15189) ;
#4090 = VERTEX_POINT('',#15195) ;
#4091 = VERTEX_POINT('',#15200) ;
#4092 = VERTEX_POINT('',#15202) ;
#4093 = VERTEX_POINT('',#15208) ;
#4094 = VERTEX_POINT('',#15210) ;
#4095 = VERTEX_POINT('',#15217) ;
#4096 = VERTEX_POINT('',#15219) ;
#4097 = VERTEX_POINT('',#15225) ;
#4098 = VERTEX_POINT('',#15227) ;
#4099 = VERTEX_POINT('',#15233) ;
#4100 = VERTEX_POINT('',#15235) ;
#4101 = VERTEX_POINT('',#15242) ;
#4102 = VERTEX_POINT('',#15243) ;
#4103 = VERTEX_POINT('',#15245) ;
#4104 = VERTEX_POINT('',#15247) ;
#4105 = VERTEX_POINT('',#15249) ;
#4106 = VERTEX_POINT('',#15251) ;
#4107 = VERTEX_POINT('',#15253) ;
#4108 = VERTEX_POINT('',#15257) ;
#4109 = VERTEX_POINT('',#15259) ;
#4110 = VERTEX_POINT('',#15263) ;
#4111 = VERTEX_POINT('',#15265) ;
#4112 = VERTEX_POINT('',#15269) ;
#4113 = VERTEX_POINT('',#15271) ;
#4114 = VERTEX_POINT('',#15273) ;
#4115 = VERTEX_POINT('',#15278) ;
#4116 = VERTEX_POINT('',#15280) ;
#4117 = VERTEX_POINT('',#15282) ;
#4118 = VERTEX_POINT('',#15284) ;
#4119 = VERTEX_POINT('',#15288) ;
#4120 = VERTEX_POINT('',#15292) ;
#4121 = VERTEX_POINT('',#15296) ;
#4122 = VERTEX_POINT('',#15299) ;
#4123 = VERTEX_POINT('',#15303) ;
#4124 = VERTEX_POINT('',#15305) ;
#4125 = VERTEX_POINT('',#15315) ;
#4126 = VERTEX_POINT('',#15317) ;
#4127 = VERTEX_POINT('',#15323) ;
#4128 = VERTEX_POINT('',#15325) ;
#4129 = VERTEX_POINT('',#15331) ;
#4130 = VERTEX_POINT('',#15333) ;
#4131 = VERTEX_POINT('',#15340) ;
#4132 = VERTEX_POINT('',#15342) ;
#4133 = VERTEX_POINT('',#15359) ;
#4134 = VERTEX_POINT('',#15361) ;
#4135 = VERTEX_POINT('',#15366) ;
#4136 = VERTEX_POINT('',#15368) ;
#4137 = VERTEX_POINT('',#15375) ;
#4138 = VERTEX_POINT('',#15377) ;
#4139 = VERTEX_POINT('',#15382) ;
#4140 = VERTEX_POINT('',#15384) ;
#4141 = EDGE_CURVE('',#3388,#3389,#2440,.T.) ;
#4142 = EDGE_CURVE('',#3390,#3388,#2441,.T.) ;
#4143 = EDGE_CURVE('',#3391,#3390,#2442,.T.) ;
#4144 = EDGE_CURVE('',#3389,#3391,#2443,.T.) ;
#4145 = EDGE_CURVE('',#3392,#3391,#2444,.T.) ;
#4146 = EDGE_CURVE('',#3393,#3392,#2445,.T.) ;
#4147 = EDGE_CURVE('',#3393,#3394,#2446,.T.) ;
#4148 = EDGE_CURVE('',#3394,#3395,#2447,.T.) ;
#4149 = EDGE_CURVE('',#3395,#3389,#2448,.T.) ;
#4150 = EDGE_CURVE('',#3396,#3390,#2449,.T.) ;
#4151 = EDGE_CURVE('',#3396,#3397,#2450,.T.) ;
#4152 = EDGE_CURVE('',#3398,#3397,#2451,.T.) ;
#4153 = EDGE_CURVE('',#3392,#3398,#2452,.T.) ;
#4154 = EDGE_CURVE('',#3399,#3388,#2453,.T.) ;
#4155 = EDGE_CURVE('',#3396,#3399,#2454,.T.) ;
#4156 = EDGE_CURVE('',#3399,#3395,#2455,.T.) ;
#4157 = EDGE_CURVE('',#3400,#3394,#2456,.T.) ;
#4158 = EDGE_CURVE('',#3397,#3400,#2457,.T.) ;
#4159 = EDGE_CURVE('',#3401,#3401,#885,.T.) ;
#4160 = EDGE_CURVE('',#3402,#3402,#886,.T.) ;
#4161 = EDGE_CURVE('',#3403,#3404,#2458,.T.) ;
#4162 = EDGE_CURVE('',#3404,#3405,#2459,.T.) ;
#4163 = EDGE_CURVE('',#3405,#3406,#2460,.T.) ;
#4164 = EDGE_CURVE('',#3406,#3403,#2461,.T.) ;
#4165 = EDGE_CURVE('',#3407,#3408,#2462,.T.) ;
#4166 = EDGE_CURVE('',#3408,#3409,#2463,.T.) ;
#4167 = EDGE_CURVE('',#3409,#3410,#2464,.T.) ;
#4168 = EDGE_CURVE('',#3410,#3407,#2465,.T.) ;
#4169 = EDGE_CURVE('',#3411,#3411,#887,.T.) ;
#4170 = EDGE_CURVE('',#3412,#3412,#888,.T.) ;
#4171 = EDGE_CURVE('',#3413,#3413,#889,.T.) ;
#4172 = EDGE_CURVE('',#3413,#3414,#2466,.T.) ;
#4173 = EDGE_CURVE('',#3414,#3414,#890,.T.) ;
#4174 = EDGE_CURVE('',#3415,#3415,#891,.T.) ;
#4175 = EDGE_CURVE('',#3415,#3416,#2467,.T.) ;
#4176 = EDGE_CURVE('',#3416,#3416,#892,.T.) ;
#4177 = EDGE_CURVE('',#3417,#3417,#893,.T.) ;
#4178 = EDGE_CURVE('',#3417,#3418,#2468,.T.) ;
#4179 = EDGE_CURVE('',#3418,#3418,#894,.T.) ;
#4180 = EDGE_CURVE('',#3419,#3420,#2469,.T.) ;
#4181 = EDGE_CURVE('',#3421,#3420,#2470,.T.) ;
#4182 = EDGE_CURVE('',#3421,#3422,#2471,.T.) ;
#4183 = EDGE_CURVE('',#3422,#3419,#2472,.T.) ;
#4184 = EDGE_CURVE('',#3422,#3423,#2473,.T.) ;
#4185 = EDGE_CURVE('',#3424,#3423,#2474,.T.) ;
#4186 = EDGE_CURVE('',#3419,#3424,#2475,.T.) ;
#4187 = EDGE_CURVE('',#3425,#3421,#2476,.T.) ;
#4188 = EDGE_CURVE('',#3423,#3425,#2477,.T.) ;
#4189 = EDGE_CURVE('',#3426,#3424,#2478,.T.) ;
#4190 = EDGE_CURVE('',#3420,#3426,#2479,.T.) ;
#4191 = EDGE_CURVE('',#3427,#3426,#2480,.T.) ;
#4192 = EDGE_CURVE('',#3428,#3427,#2481,.T.) ;
#4193 = EDGE_CURVE('',#3429,#3428,#2482,.T.) ;
#4194 = EDGE_CURVE('',#3429,#3430,#2483,.T.) ;
#4195 = EDGE_CURVE('',#3425,#3430,#2484,.T.) ;
#4196 = EDGE_CURVE('',#3431,#3431,#895,.T.) ;
#4197 = EDGE_CURVE('',#3431,#3432,#2485,.T.) ;
#4198 = EDGE_CURVE('',#3432,#3432,#896,.T.) ;
#4199 = EDGE_CURVE('',#3433,#3434,#2486,.T.) ;
#4200 = EDGE_CURVE('',#3434,#3435,#2487,.T.) ;
#4201 = EDGE_CURVE('',#3435,#3436,#2488,.T.) ;
#4202 = EDGE_CURVE('',#3433,#3436,#2489,.T.) ;
#4203 = EDGE_CURVE('',#3435,#3437,#2490,.T.) ;
#4204 = EDGE_CURVE('',#3438,#3437,#2491,.T.) ;
#4205 = EDGE_CURVE('',#3436,#3438,#2492,.T.) ;
#4206 = EDGE_CURVE('',#3434,#3439,#2493,.T.) ;
#4207 = EDGE_CURVE('',#3437,#3439,#2494,.T.) ;
#4208 = EDGE_CURVE('',#3440,#3433,#2495,.T.) ;
#4209 = EDGE_CURVE('',#3439,#3440,#2496,.T.) ;
#4210 = EDGE_CURVE('',#3441,#3438,#2497,.T.) ;
#4211 = EDGE_CURVE('',#3442,#3441,#2498,.T.) ;
#4212 = EDGE_CURVE('',#3443,#3442,#2499,.T.) ;
#4213 = EDGE_CURVE('',#3443,#3444,#2500,.T.) ;
#4214 = EDGE_CURVE('',#3440,#3444,#2501,.T.) ;
#4215 = EDGE_CURVE('',#3445,#3445,#897,.T.) ;
#4216 = EDGE_CURVE('',#3445,#3446,#2502,.T.) ;
#4217 = EDGE_CURVE('',#3446,#3446,#898,.T.) ;
#4218 = EDGE_CURVE('',#3447,#3447,#899,.T.) ;
#4219 = EDGE_CURVE('',#3447,#3401,#2503,.T.) ;
#4220 = EDGE_CURVE('',#3448,#3448,#900,.T.) ;
#4221 = EDGE_CURVE('',#3448,#3449,#2504,.T.) ;
#4222 = EDGE_CURVE('',#3449,#3449,#901,.T.) ;
#4223 = EDGE_CURVE('',#3450,#3450,#902,.T.) ;
#4224 = EDGE_CURVE('',#3450,#3412,#2505,.T.) ;
#4225 = EDGE_CURVE('',#3451,#3451,#903,.T.) ;
#4226 = EDGE_CURVE('',#3451,#3452,#2506,.T.) ;
#4227 = EDGE_CURVE('',#3452,#3452,#904,.T.) ;
#4228 = EDGE_CURVE('',#3453,#3453,#905,.T.) ;
#4229 = EDGE_CURVE('',#3453,#3402,#2507,.T.) ;
#4230 = EDGE_CURVE('',#3454,#3454,#906,.T.) ;
#4231 = EDGE_CURVE('',#3454,#3455,#2508,.T.) ;
#4232 = EDGE_CURVE('',#3455,#3455,#907,.T.) ;
#4233 = EDGE_CURVE('',#3456,#3456,#908,.T.) ;
#4234 = EDGE_CURVE('',#3456,#3457,#2509,.T.) ;
#4235 = EDGE_CURVE('',#3457,#3457,#909,.T.) ;
#4236 = EDGE_CURVE('',#3458,#3459,#2510,.T.) ;
#4237 = EDGE_CURVE('',#3459,#3460,#2511,.T.) ;
#4238 = EDGE_CURVE('',#3460,#3461,#2512,.T.) ;
#4239 = EDGE_CURVE('',#3461,#3458,#2513,.T.) ;
#4240 = EDGE_CURVE('',#3461,#3404,#2514,.T.) ;
#4241 = EDGE_CURVE('',#3458,#3403,#2515,.T.) ;
#4242 = EDGE_CURVE('',#3460,#3405,#2516,.T.) ;
#4243 = EDGE_CURVE('',#3459,#3406,#2517,.T.) ;
#4244 = EDGE_CURVE('',#3462,#3463,#2518,.T.) ;
#4245 = EDGE_CURVE('',#3463,#3464,#2519,.T.) ;
#4246 = EDGE_CURVE('',#3464,#3465,#2520,.T.) ;
#4247 = EDGE_CURVE('',#3465,#3462,#2521,.T.) ;
#4248 = EDGE_CURVE('',#3465,#3408,#2522,.T.) ;
#4249 = EDGE_CURVE('',#3462,#3407,#2523,.T.) ;
#4250 = EDGE_CURVE('',#3464,#3409,#2524,.T.) ;
#4251 = EDGE_CURVE('',#3463,#3410,#2525,.T.) ;
#4252 = EDGE_CURVE('',#3466,#3466,#910,.T.) ;
#4253 = EDGE_CURVE('',#3466,#3411,#2526,.T.) ;
#4254 = EDGE_CURVE('',#3398,#3467,#2527,.T.) ;
#4255 = EDGE_CURVE('',#3467,#3400,#2528,.T.) ;
#4256 = EDGE_CURVE('',#3467,#3393,#2529,.T.) ;
#4257 = EDGE_CURVE('',#3428,#3443,#2530,.T.) ;
#4258 = EDGE_CURVE('',#3442,#3429,#2531,.T.) ;
#4259 = EDGE_CURVE('',#3444,#3427,#2532,.T.) ;
#4260 = EDGE_CURVE('',#3430,#3441,#2533,.T.) ;
#4261 = EDGE_CURVE('',#3468,#3469,#2534,.T.) ;
#4262 = EDGE_CURVE('',#3468,#3470,#911,.T.) ;
#4263 = EDGE_CURVE('',#3471,#3470,#2535,.T.) ;
#4264 = EDGE_CURVE('',#3469,#3471,#912,.T.) ;
#4265 = EDGE_CURVE('',#3472,#3468,#2536,.T.) ;
#4266 = EDGE_CURVE('',#3473,#3472,#913,.T.) ;
#4267 = EDGE_CURVE('',#3470,#3473,#2537,.T.) ;
#4268 = EDGE_CURVE('',#3474,#3474,#914,.T.) ;
#4269 = EDGE_CURVE('',#3475,#3472,#2538,.T.) ;
#4270 = EDGE_CURVE('',#3476,#3475,#915,.T.) ;
#4271 = EDGE_CURVE('',#3473,#3476,#2539,.T.) ;
#4272 = EDGE_CURVE('',#3477,#3469,#2540,.T.) ;
#4273 = EDGE_CURVE('',#3478,#3477,#2541,.T.) ;
#4274 = EDGE_CURVE('',#3479,#3478,#2542,.T.) ;
#4275 = EDGE_CURVE('',#3479,#3480,#2543,.T.) ;
#4276 = EDGE_CURVE('',#3475,#3480,#2544,.T.) ;
#4277 = EDGE_CURVE('',#3481,#3481,#916,.T.) ;
#4278 = EDGE_CURVE('',#3471,#3477,#2545,.T.) ;
#4279 = EDGE_CURVE('',#3474,#3482,#2546,.T.) ;
#4280 = EDGE_CURVE('',#3482,#3482,#917,.T.) ;
#4281 = EDGE_CURVE('',#3483,#3484,#2547,.T.) ;
#4282 = EDGE_CURVE('',#3485,#3483,#918,.T.) ;
#4283 = EDGE_CURVE('',#3486,#3485,#2548,.T.) ;
#4284 = EDGE_CURVE('',#3486,#3484,#919,.T.) ;
#4285 = EDGE_CURVE('',#3487,#3488,#2549,.T.) ;
#4286 = EDGE_CURVE('',#3487,#3489,#920,.T.) ;
#4287 = EDGE_CURVE('',#3490,#3489,#2550,.T.) ;
#4288 = EDGE_CURVE('',#3488,#3490,#921,.T.) ;
#4289 = EDGE_CURVE('',#3484,#3487,#2551,.T.) ;
#4290 = EDGE_CURVE('',#3489,#3486,#2552,.T.) ;
#4291 = EDGE_CURVE('',#3491,#3491,#922,.T.) ;
#4292 = EDGE_CURVE('',#3490,#3476,#2553,.T.) ;
#4293 = EDGE_CURVE('',#3492,#3485,#2554,.T.) ;
#4294 = EDGE_CURVE('',#3493,#3492,#2555,.T.) ;
#4295 = EDGE_CURVE('',#3478,#3493,#2556,.T.) ;
#4296 = EDGE_CURVE('',#3483,#3492,#2557,.T.) ;
#4297 = EDGE_CURVE('',#3480,#3494,#2558,.T.) ;
#4298 = EDGE_CURVE('',#3494,#3488,#2559,.T.) ;
#4299 = EDGE_CURVE('',#3491,#3495,#2560,.T.) ;
#4300 = EDGE_CURVE('',#3495,#3495,#923,.T.) ;
#4301 = EDGE_CURVE('',#3496,#3496,#924,.T.) ;
#4302 = EDGE_CURVE('',#3496,#3481,#2561,.T.) ;
#4303 = EDGE_CURVE('',#3493,#3497,#2562,.T.) ;
#4304 = EDGE_CURVE('',#3497,#3479,#2563,.T.) ;
#4305 = EDGE_CURVE('',#3497,#3494,#2564,.T.) ;
#4306 = EDGE_CURVE('',#3498,#3498,#925,.T.) ;
#4307 = EDGE_CURVE('',#3498,#3499,#2565,.T.) ;
#4308 = EDGE_CURVE('',#3499,#3499,#926,.T.) ;
#4309 = EDGE_CURVE('',#3500,#3501,#2566,.T.) ;
#4310 = EDGE_CURVE('',#3500,#3502,#2567,.T.) ;
#4311 = EDGE_CURVE('',#3502,#3503,#2568,.T.) ;
#4312 = EDGE_CURVE('',#3501,#3503,#2569,.T.) ;
#4313 = EDGE_CURVE('',#3501,#3504,#2570,.T.) ;
#4314 = EDGE_CURVE('',#3503,#3505,#2571,.T.) ;
#4315 = EDGE_CURVE('',#3504,#3505,#2572,.T.) ;
#4316 = EDGE_CURVE('',#3506,#3502,#2573,.T.) ;
#4317 = EDGE_CURVE('',#3505,#3506,#2574,.T.) ;
#4318 = EDGE_CURVE('',#3504,#3507,#2575,.T.) ;
#4319 = EDGE_CURVE('',#3507,#3506,#2576,.T.) ;
#4320 = EDGE_CURVE('',#3507,#3500,#2577,.T.) ;
#4321 = EDGE_CURVE('',#3508,#3509,#2578,.T.) ;
#4322 = EDGE_CURVE('',#3508,#3510,#2579,.T.) ;
#4323 = EDGE_CURVE('',#3510,#3511,#2580,.T.) ;
#4324 = EDGE_CURVE('',#3509,#3511,#2581,.T.) ;
#4325 = EDGE_CURVE('',#3509,#3512,#2582,.T.) ;
#4326 = EDGE_CURVE('',#3511,#3513,#2583,.T.) ;
#4327 = EDGE_CURVE('',#3512,#3513,#2584,.T.) ;
#4328 = EDGE_CURVE('',#3514,#3510,#2585,.T.) ;
#4329 = EDGE_CURVE('',#3513,#3514,#2586,.T.) ;
#4330 = EDGE_CURVE('',#3512,#3515,#2587,.T.) ;
#4331 = EDGE_CURVE('',#3515,#3514,#2588,.T.) ;
#4332 = EDGE_CURVE('',#3515,#3508,#2589,.T.) ;
#4333 = EDGE_CURVE('',#3516,#3517,#2590,.T.) ;
#4334 = EDGE_CURVE('',#3516,#3518,#2591,.T.) ;
#4335 = EDGE_CURVE('',#3518,#3519,#2592,.T.) ;
#4336 = EDGE_CURVE('',#3517,#3519,#2593,.T.) ;
#4337 = EDGE_CURVE('',#3517,#3520,#2594,.T.) ;
#4338 = EDGE_CURVE('',#3519,#3521,#2595,.T.) ;
#4339 = EDGE_CURVE('',#3520,#3521,#2596,.T.) ;
#4340 = EDGE_CURVE('',#3522,#3518,#2597,.T.) ;
#4341 = EDGE_CURVE('',#3521,#3522,#2598,.T.) ;
#4342 = EDGE_CURVE('',#3520,#3523,#2599,.T.) ;
#4343 = EDGE_CURVE('',#3523,#3522,#2600,.T.) ;
#4344 = EDGE_CURVE('',#3523,#3516,#2601,.T.) ;
#4345 = EDGE_CURVE('',#3524,#3524,#927,.T.) ;
#4346 = EDGE_CURVE('',#3524,#3525,#2602,.T.) ;
#4347 = EDGE_CURVE('',#3525,#3525,#928,.T.) ;
#4348 = EDGE_CURVE('',#3526,#3526,#929,.T.) ;
#4349 = EDGE_CURVE('',#3526,#3527,#2603,.T.) ;
#4350 = EDGE_CURVE('',#3527,#3527,#930,.T.) ;
#4351 = EDGE_CURVE('',#3528,#3528,#931,.T.) ;
#4352 = EDGE_CURVE('',#3529,#3529,#932,.T.) ;
#4353 = EDGE_CURVE('',#3529,#3528,#2604,.T.) ;
#4354 = EDGE_CURVE('',#3530,#3530,#933,.T.) ;
#4355 = EDGE_CURVE('',#3530,#3531,#2605,.T.) ;
#4356 = EDGE_CURVE('',#3531,#3531,#934,.T.) ;
#4357 = EDGE_CURVE('',#3532,#3532,#935,.T.) ;
#4358 = EDGE_CURVE('',#3533,#3533,#936,.T.) ;
#4359 = EDGE_CURVE('',#3533,#3532,#2606,.T.) ;
#4360 = EDGE_CURVE('',#3534,#3534,#937,.T.) ;
#4361 = EDGE_CURVE('',#3534,#3535,#2607,.T.) ;
#4362 = EDGE_CURVE('',#3535,#3535,#938,.T.) ;
#4363 = EDGE_CURVE('',#3536,#3536,#939,.T.) ;
#4364 = EDGE_CURVE('',#3536,#3537,#2608,.T.) ;
#4365 = EDGE_CURVE('',#3537,#3537,#940,.T.) ;
#4366 = EDGE_CURVE('',#3538,#3538,#941,.T.) ;
#4367 = EDGE_CURVE('',#3538,#3539,#2609,.T.) ;
#4368 = EDGE_CURVE('',#3539,#3539,#942,.T.) ;
#4369 = EDGE_CURVE('',#3540,#3540,#943,.T.) ;
#4370 = EDGE_CURVE('',#3540,#3541,#2610,.T.) ;
#4371 = EDGE_CURVE('',#3541,#3541,#944,.T.) ;
#4372 = EDGE_CURVE('',#3542,#3542,#945,.T.) ;
#4373 = EDGE_CURVE('',#3542,#3543,#946,.T.) ;
#4374 = EDGE_CURVE('',#3544,#3544,#947,.T.) ;
#4375 = EDGE_CURVE('',#3544,#3542,#2611,.T.) ;
#4376 = EDGE_CURVE('',#3545,#3545,#948,.T.) ;
#4377 = EDGE_CURVE('',#3545,#3546,#2612,.T.) ;
#4378 = EDGE_CURVE('',#3546,#3546,#949,.T.) ;
#4379 = EDGE_CURVE('',#3547,#3547,#950,.T.) ;
#4380 = EDGE_CURVE('',#3547,#3548,#2613,.T.) ;
#4381 = EDGE_CURVE('',#3548,#3548,#951,.T.) ;
#4382 = EDGE_CURVE('',#3549,#3549,#952,.T.) ;
#4383 = EDGE_CURVE('',#3549,#3550,#2614,.T.) ;
#4384 = EDGE_CURVE('',#3550,#3550,#953,.T.) ;
#4385 = EDGE_CURVE('',#3551,#3551,#954,.T.) ;
#4386 = EDGE_CURVE('',#3551,#3552,#2615,.T.) ;
#4387 = EDGE_CURVE('',#3552,#3552,#955,.T.) ;
#4388 = EDGE_CURVE('',#3553,#3553,#956,.T.) ;
#4389 = EDGE_CURVE('',#3553,#3554,#2616,.T.) ;
#4390 = EDGE_CURVE('',#3554,#3554,#957,.T.) ;
#4391 = EDGE_CURVE('',#3555,#3555,#958,.T.) ;
#4392 = EDGE_CURVE('',#3555,#3556,#2617,.T.) ;
#4393 = EDGE_CURVE('',#3556,#3556,#959,.T.) ;
#4394 = EDGE_CURVE('',#3557,#3558,#2618,.T.) ;
#4395 = EDGE_CURVE('',#3559,#3557,#2619,.T.) ;
#4396 = EDGE_CURVE('',#3560,#3559,#2620,.T.) ;
#4397 = EDGE_CURVE('',#3558,#3560,#2621,.T.) ;
#4398 = EDGE_CURVE('',#3561,#3562,#960,.T.) ;
#4399 = EDGE_CURVE('',#3561,#3563,#2622,.T.) ;
#4400 = EDGE_CURVE('',#3563,#3562,#2623,.T.) ;
#4401 = EDGE_CURVE('',#3564,#3561,#2624,.T.) ;
#4402 = EDGE_CURVE('',#3565,#3564,#2625,.T.) ;
#4403 = EDGE_CURVE('',#3563,#3565,#2626,.T.) ;
#4404 = EDGE_CURVE('',#3566,#3564,#961,.T.) ;
#4405 = EDGE_CURVE('',#3566,#3565,#2627,.T.) ;
#4406 = EDGE_CURVE('',#3567,#3557,#962,.T.) ;
#4407 = EDGE_CURVE('',#3567,#3559,#2628,.T.) ;
#4408 = EDGE_CURVE('',#3558,#3568,#963,.T.) ;
#4409 = EDGE_CURVE('',#3560,#3568,#2629,.T.) ;
#4410 = EDGE_CURVE('',#3568,#3567,#2630,.T.) ;
#4411 = EDGE_CURVE('',#3562,#3566,#2631,.T.) ;
#4412 = EDGE_CURVE('',#3569,#3569,#964,.T.) ;
#4413 = EDGE_CURVE('',#3569,#3570,#2632,.T.) ;
#4414 = EDGE_CURVE('',#3570,#3570,#965,.T.) ;
#4415 = EDGE_CURVE('',#3571,#3572,#966,.T.) ;
#4416 = EDGE_CURVE('',#3572,#3571,#967,.T.) ;
#4417 = EDGE_CURVE('',#3573,#3571,#2633,.T.) ;
#4418 = EDGE_CURVE('',#3574,#3573,#968,.T.) ;
#4419 = EDGE_CURVE('',#3574,#3575,#2634,.T.) ;
#4420 = EDGE_CURVE('',#3575,#3575,#969,.T.) ;
#4421 = EDGE_CURVE('',#3576,#3574,#970,.T.) ;
#4422 = EDGE_CURVE('',#3572,#3576,#2635,.T.) ;
#4423 = EDGE_CURVE('',#3577,#3577,#971,.T.) ;
#4424 = EDGE_CURVE('',#3577,#3578,#2636,.T.) ;
#4425 = EDGE_CURVE('',#3573,#3578,#972,.T.) ;
#4426 = EDGE_CURVE('',#3578,#3576,#973,.T.) ;
#4427 = EDGE_CURVE('',#3579,#3579,#974,.T.) ;
#4428 = EDGE_CURVE('',#3579,#3580,#2637,.T.) ;
#4429 = EDGE_CURVE('',#3580,#3580,#975,.T.) ;
#4430 = EDGE_CURVE('',#3581,#3582,#976,.T.) ;
#4431 = EDGE_CURVE('',#3583,#3584,#977,.T.) ;
#4432 = EDGE_CURVE('',#3584,#3583,#978,.T.) ;
#4433 = EDGE_CURVE('',#3583,#3584,#13,.T.) ;
#4434 = EDGE_CURVE('',#3585,#3585,#979,.T.) ;
#4435 = EDGE_CURVE('',#3586,#3586,#980,.T.) ;
#4436 = EDGE_CURVE('',#3587,#3588,#11,.T.) ;
#4437 = EDGE_CURVE('',#3587,#3588,#981,.T.) ;
#4438 = EDGE_CURVE('',#3589,#3590,#14,.T.) ;
#4439 = EDGE_CURVE('',#3591,#3590,#982,.T.) ;
#4440 = EDGE_CURVE('',#3591,#3585,#2638,.T.) ;
#4441 = EDGE_CURVE('',#3589,#3591,#983,.T.) ;
#4442 = EDGE_CURVE('',#3592,#3592,#984,.T.) ;
#4443 = EDGE_CURVE('',#3593,#3593,#985,.T.) ;
#4444 = EDGE_CURVE('',#3594,#3595,#12,.T.) ;
#4445 = EDGE_CURVE('',#3595,#3594,#986,.T.) ;
#4446 = EDGE_CURVE('',#3592,#3596,#2639,.T.) ;
#4447 = EDGE_CURVE('',#3590,#3596,#987,.T.) ;
#4448 = EDGE_CURVE('',#3596,#3589,#988,.T.) ;
#4449 = EDGE_CURVE('',#3587,#3597,#989,.T.) ;
#4450 = EDGE_CURVE('',#3597,#3593,#2640,.T.) ;
#4451 = EDGE_CURVE('',#3597,#3588,#990,.T.) ;
#4452 = EDGE_CURVE('',#3586,#3598,#2641,.T.) ;
#4453 = EDGE_CURVE('',#3598,#3594,#991,.T.) ;
#4454 = EDGE_CURVE('',#3595,#3598,#992,.T.) ;
#4455 = EDGE_CURVE('',#3599,#3599,#993,.T.) ;
#4456 = EDGE_CURVE('',#3599,#3600,#2642,.T.) ;
#4457 = EDGE_CURVE('',#3600,#3600,#994,.T.) ;
#4458 = EDGE_CURVE('',#3601,#3601,#995,.T.) ;
#4459 = EDGE_CURVE('',#3601,#3602,#2643,.T.) ;
#4460 = EDGE_CURVE('',#3602,#3602,#996,.T.) ;
#4461 = EDGE_CURVE('',#3603,#3603,#997,.T.) ;
#4462 = EDGE_CURVE('',#3603,#3604,#2644,.T.) ;
#4463 = EDGE_CURVE('',#3604,#3604,#998,.T.) ;
#4464 = EDGE_CURVE('',#3605,#3605,#999,.T.) ;
#4465 = EDGE_CURVE('',#3605,#3606,#2645,.T.) ;
#4466 = EDGE_CURVE('',#3606,#3606,#1000,.T.) ;
#4467 = EDGE_CURVE('',#3607,#3607,#1001,.T.) ;
#4468 = EDGE_CURVE('',#3607,#3608,#2646,.T.) ;
#4469 = EDGE_CURVE('',#3608,#3608,#1002,.T.) ;
#4470 = EDGE_CURVE('',#3609,#3609,#1003,.T.) ;
#4471 = EDGE_CURVE('',#3609,#3610,#2647,.T.) ;
#4472 = EDGE_CURVE('',#3610,#3610,#1004,.T.) ;
#4473 = EDGE_CURVE('',#3611,#3611,#1005,.T.) ;
#4474 = EDGE_CURVE('',#3611,#3612,#2648,.T.) ;
#4475 = EDGE_CURVE('',#3612,#3612,#1006,.T.) ;
#4476 = EDGE_CURVE('',#3613,#3613,#1007,.T.) ;
#4477 = EDGE_CURVE('',#3613,#3614,#2649,.T.) ;
#4478 = EDGE_CURVE('',#3614,#3614,#1008,.T.) ;
#4479 = EDGE_CURVE('',#3615,#3616,#2650,.T.) ;
#4480 = EDGE_CURVE('',#3616,#3617,#2651,.T.) ;
#4481 = EDGE_CURVE('',#3617,#3618,#2652,.T.) ;
#4482 = EDGE_CURVE('',#3618,#3615,#2653,.T.) ;
#4483 = EDGE_CURVE('',#3619,#3618,#2654,.T.) ;
#4484 = EDGE_CURVE('',#3620,#3617,#2655,.T.) ;
#4485 = EDGE_CURVE('',#3619,#3620,#2656,.T.) ;
#4486 = EDGE_CURVE('',#3621,#3622,#2657,.T.) ;
#4487 = EDGE_CURVE('',#3621,#3616,#2658,.T.) ;
#4488 = EDGE_CURVE('',#3622,#3615,#2659,.T.) ;
#4489 = EDGE_CURVE('',#3623,#3621,#2660,.T.) ;
#4490 = EDGE_CURVE('',#3623,#3624,#1009,.T.) ;
#4491 = EDGE_CURVE('',#3625,#3624,#2661,.T.) ;
#4492 = EDGE_CURVE('',#3626,#3625,#2662,.T.) ;
#4493 = EDGE_CURVE('',#3627,#3626,#2663,.T.) ;
#4494 = EDGE_CURVE('',#3627,#3628,#1010,.T.) ;
#4495 = EDGE_CURVE('',#3620,#3628,#2664,.T.) ;
#4496 = EDGE_CURVE('',#3629,#3629,#1011,.T.) ;
#4497 = EDGE_CURVE('',#3622,#3630,#2665,.T.) ;
#4498 = EDGE_CURVE('',#3630,#3623,#2666,.T.) ;
#4499 = EDGE_CURVE('',#3629,#3631,#2667,.T.) ;
#4500 = EDGE_CURVE('',#3631,#3631,#1012,.T.) ;
#4501 = EDGE_CURVE('',#3632,#3630,#1013,.T.) ;
#4502 = EDGE_CURVE('',#3624,#3632,#2668,.T.) ;
#4503 = EDGE_CURVE('',#3628,#3633,#2669,.T.) ;
#4504 = EDGE_CURVE('',#3634,#3627,#2670,.T.) ;
#4505 = EDGE_CURVE('',#3633,#3634,#1014,.T.) ;
#4506 = EDGE_CURVE('',#3626,#3635,#2671,.T.) ;
#4507 = EDGE_CURVE('',#3635,#3634,#2672,.T.) ;
#4508 = EDGE_CURVE('',#3633,#3619,#2673,.T.) ;
#4509 = EDGE_CURVE('',#3635,#3636,#2674,.T.) ;
#4510 = EDGE_CURVE('',#3632,#3636,#2675,.T.) ;
#4511 = EDGE_CURVE('',#3636,#3625,#2676,.T.) ;
#4512 = EDGE_CURVE('',#3637,#3637,#1015,.T.) ;
#4513 = EDGE_CURVE('',#3638,#3638,#1016,.T.) ;
#4514 = EDGE_CURVE('',#3637,#3639,#2677,.T.) ;
#4515 = EDGE_CURVE('',#3639,#3639,#1017,.T.) ;
#4516 = EDGE_CURVE('',#3640,#3640,#1018,.T.) ;
#4517 = EDGE_CURVE('',#3640,#3638,#2678,.T.) ;
#4518 = EDGE_CURVE('',#3641,#3642,#1019,.T.) ;
#4519 = EDGE_CURVE('',#3642,#3641,#1020,.T.) ;
#4520 = EDGE_CURVE('',#3643,#3644,#1021,.T.) ;
#4521 = EDGE_CURVE('',#3644,#3645,#1022,.T.) ;
#4522 = EDGE_CURVE('',#3645,#3643,#1023,.T.) ;
#4523 = EDGE_CURVE('',#3646,#3647,#1024,.T.) ;
#4524 = EDGE_CURVE('',#3647,#3648,#1025,.T.) ;
#4525 = EDGE_CURVE('',#3648,#3649,#1026,.T.) ;
#4526 = EDGE_CURVE('',#3649,#3646,#1027,.T.) ;
#4527 = EDGE_CURVE('',#3650,#3651,#1028,.T.) ;
#4528 = EDGE_CURVE('',#3651,#3652,#1029,.T.) ;
#4529 = EDGE_CURVE('',#3652,#3653,#1030,.T.) ;
#4530 = EDGE_CURVE('',#3653,#3650,#1031,.T.) ;
#4531 = EDGE_CURVE('',#3654,#3655,#1032,.T.) ;
#4532 = EDGE_CURVE('',#3655,#3656,#1033,.T.) ;
#4533 = EDGE_CURVE('',#3656,#3657,#1034,.T.) ;
#4534 = EDGE_CURVE('',#3657,#3654,#1035,.T.) ;
#4535 = EDGE_CURVE('',#3658,#3659,#1036,.T.) ;
#4536 = EDGE_CURVE('',#3659,#3660,#1037,.T.) ;
#4537 = EDGE_CURVE('',#3660,#3658,#1038,.T.) ;
#4538 = EDGE_CURVE('',#3661,#3662,#1039,.T.) ;
#4539 = EDGE_CURVE('',#3662,#3661,#1040,.T.) ;
#4540 = EDGE_CURVE('',#3663,#3664,#1041,.T.) ;
#4541 = EDGE_CURVE('',#3664,#3663,#1042,.T.) ;
#4542 = EDGE_CURVE('',#3665,#3666,#1043,.T.) ;
#4543 = EDGE_CURVE('',#3666,#3665,#1044,.T.) ;
#4544 = EDGE_CURVE('',#3667,#3668,#1045,.T.) ;
#4545 = EDGE_CURVE('',#3668,#3669,#1046,.T.) ;
#4546 = EDGE_CURVE('',#3669,#3667,#1047,.T.) ;
#4547 = EDGE_CURVE('',#3670,#3671,#1048,.T.) ;
#4548 = EDGE_CURVE('',#3671,#3672,#1049,.T.) ;
#4549 = EDGE_CURVE('',#3672,#3673,#1050,.T.) ;
#4550 = EDGE_CURVE('',#3673,#3670,#1051,.T.) ;
#4551 = EDGE_CURVE('',#3674,#3675,#1052,.T.) ;
#4552 = EDGE_CURVE('',#3675,#3676,#1053,.T.) ;
#4553 = EDGE_CURVE('',#3676,#3677,#1054,.T.) ;
#4554 = EDGE_CURVE('',#3677,#3674,#1055,.T.) ;
#4555 = EDGE_CURVE('',#3678,#3679,#1056,.T.) ;
#4556 = EDGE_CURVE('',#3679,#3680,#1057,.T.) ;
#4557 = EDGE_CURVE('',#3680,#3681,#1058,.T.) ;
#4558 = EDGE_CURVE('',#3681,#3678,#1059,.T.) ;
#4559 = EDGE_CURVE('',#3682,#3683,#1060,.T.) ;
#4560 = EDGE_CURVE('',#3683,#3684,#1061,.T.) ;
#4561 = EDGE_CURVE('',#3684,#3682,#1062,.T.) ;
#4562 = EDGE_CURVE('',#3685,#3686,#1063,.T.) ;
#4563 = EDGE_CURVE('',#3686,#3685,#1064,.T.) ;
#4564 = EDGE_CURVE('',#3687,#3688,#1065,.T.) ;
#4565 = EDGE_CURVE('',#3688,#3687,#1066,.T.) ;
#4566 = EDGE_CURVE('',#3689,#3690,#1067,.T.) ;
#4567 = EDGE_CURVE('',#3690,#3689,#1068,.T.) ;
#4568 = EDGE_CURVE('',#3691,#3692,#1069,.T.) ;
#4569 = EDGE_CURVE('',#3692,#3693,#1070,.T.) ;
#4570 = EDGE_CURVE('',#3693,#3691,#1071,.T.) ;
#4571 = EDGE_CURVE('',#3694,#3695,#1072,.T.) ;
#4572 = EDGE_CURVE('',#3695,#3696,#1073,.T.) ;
#4573 = EDGE_CURVE('',#3696,#3697,#1074,.T.) ;
#4574 = EDGE_CURVE('',#3697,#3694,#1075,.T.) ;
#4575 = EDGE_CURVE('',#3698,#3699,#1076,.T.) ;
#4576 = EDGE_CURVE('',#3699,#3700,#1077,.T.) ;
#4577 = EDGE_CURVE('',#3700,#3701,#1078,.T.) ;
#4578 = EDGE_CURVE('',#3701,#3698,#1079,.T.) ;
#4579 = EDGE_CURVE('',#3702,#3703,#1080,.T.) ;
#4580 = EDGE_CURVE('',#3703,#3704,#1081,.T.) ;
#4581 = EDGE_CURVE('',#3704,#3705,#1082,.T.) ;
#4582 = EDGE_CURVE('',#3705,#3702,#1083,.T.) ;
#4583 = EDGE_CURVE('',#3706,#3707,#1084,.T.) ;
#4584 = EDGE_CURVE('',#3707,#3708,#1085,.T.) ;
#4585 = EDGE_CURVE('',#3708,#3706,#1086,.T.) ;
#4586 = EDGE_CURVE('',#3709,#3710,#1087,.T.) ;
#4587 = EDGE_CURVE('',#3710,#3709,#1088,.T.) ;
#4588 = EDGE_CURVE('',#3711,#3712,#1089,.T.) ;
#4589 = EDGE_CURVE('',#3712,#3711,#1090,.T.) ;
#4590 = EDGE_CURVE('',#3713,#3714,#1091,.T.) ;
#4591 = EDGE_CURVE('',#3714,#3713,#1092,.T.) ;
#4592 = EDGE_CURVE('',#3715,#3716,#1093,.T.) ;
#4593 = EDGE_CURVE('',#3716,#3717,#1094,.T.) ;
#4594 = EDGE_CURVE('',#3717,#3715,#1095,.T.) ;
#4595 = EDGE_CURVE('',#3718,#3719,#1096,.T.) ;
#4596 = EDGE_CURVE('',#3719,#3720,#1097,.T.) ;
#4597 = EDGE_CURVE('',#3720,#3721,#1098,.T.) ;
#4598 = EDGE_CURVE('',#3721,#3718,#1099,.T.) ;
#4599 = EDGE_CURVE('',#3722,#3723,#1100,.T.) ;
#4600 = EDGE_CURVE('',#3723,#3724,#1101,.T.) ;
#4601 = EDGE_CURVE('',#3724,#3725,#1102,.T.) ;
#4602 = EDGE_CURVE('',#3725,#3722,#1103,.T.) ;
#4603 = EDGE_CURVE('',#3726,#3727,#1104,.T.) ;
#4604 = EDGE_CURVE('',#3727,#3728,#1105,.T.) ;
#4605 = EDGE_CURVE('',#3728,#3729,#1106,.T.) ;
#4606 = EDGE_CURVE('',#3729,#3726,#1107,.T.) ;
#4607 = EDGE_CURVE('',#3730,#3731,#1108,.T.) ;
#4608 = EDGE_CURVE('',#3731,#3732,#1109,.T.) ;
#4609 = EDGE_CURVE('',#3732,#3730,#1110,.T.) ;
#4610 = EDGE_CURVE('',#3733,#3734,#1111,.T.) ;
#4611 = EDGE_CURVE('',#3734,#3733,#1112,.T.) ;
#4612 = EDGE_CURVE('',#3735,#3736,#1113,.T.) ;
#4613 = EDGE_CURVE('',#3736,#3735,#1114,.T.) ;
#4614 = EDGE_CURVE('',#3737,#3738,#1115,.T.) ;
#4615 = EDGE_CURVE('',#3738,#3737,#1116,.T.) ;
#4616 = EDGE_CURVE('',#3739,#3740,#1117,.T.) ;
#4617 = EDGE_CURVE('',#3740,#3741,#1118,.T.) ;
#4618 = EDGE_CURVE('',#3741,#3739,#1119,.T.) ;
#4619 = EDGE_CURVE('',#3742,#3743,#1120,.T.) ;
#4620 = EDGE_CURVE('',#3743,#3744,#1121,.T.) ;
#4621 = EDGE_CURVE('',#3744,#3745,#1122,.T.) ;
#4622 = EDGE_CURVE('',#3745,#3742,#1123,.T.) ;
#4623 = EDGE_CURVE('',#3746,#3747,#1124,.T.) ;
#4624 = EDGE_CURVE('',#3747,#3748,#1125,.T.) ;
#4625 = EDGE_CURVE('',#3748,#3749,#1126,.T.) ;
#4626 = EDGE_CURVE('',#3749,#3746,#1127,.T.) ;
#4627 = EDGE_CURVE('',#3750,#3751,#1128,.T.) ;
#4628 = EDGE_CURVE('',#3751,#3752,#1129,.T.) ;
#4629 = EDGE_CURVE('',#3752,#3753,#1130,.T.) ;
#4630 = EDGE_CURVE('',#3753,#3750,#1131,.T.) ;
#4631 = EDGE_CURVE('',#3754,#3755,#1132,.T.) ;
#4632 = EDGE_CURVE('',#3755,#3756,#1133,.T.) ;
#4633 = EDGE_CURVE('',#3756,#3754,#1134,.T.) ;
#4634 = EDGE_CURVE('',#3757,#3758,#1135,.T.) ;
#4635 = EDGE_CURVE('',#3758,#3757,#1136,.T.) ;
#4636 = EDGE_CURVE('',#3759,#3759,#1137,.T.) ;
#4637 = EDGE_CURVE('',#3759,#3760,#2679,.T.) ;
#4638 = EDGE_CURVE('',#3761,#3760,#15,.T.) ;
#4639 = EDGE_CURVE('',#3642,#3761,#16,.T.) ;
#4640 = EDGE_CURVE('',#3760,#3641,#17,.T.) ;
#4641 = EDGE_CURVE('',#3761,#3762,#2680,.T.) ;
#4642 = EDGE_CURVE('',#3644,#3762,#18,.T.) ;
#4643 = EDGE_CURVE('',#3762,#3643,#19,.T.) ;
#4644 = EDGE_CURVE('',#3645,#3647,#2681,.T.) ;
#4645 = EDGE_CURVE('',#3648,#3646,#20,.T.) ;
#4646 = EDGE_CURVE('',#3649,#3651,#2682,.T.) ;
#4647 = EDGE_CURVE('',#3652,#3650,#21,.T.) ;
#4648 = EDGE_CURVE('',#3653,#3655,#2683,.T.) ;
#4649 = EDGE_CURVE('',#3656,#3654,#22,.T.) ;
#4650 = EDGE_CURVE('',#3657,#3659,#2684,.T.) ;
#4651 = EDGE_CURVE('',#3763,#3658,#23,.T.) ;
#4652 = EDGE_CURVE('',#3660,#3763,#24,.T.) ;
#4653 = EDGE_CURVE('',#3763,#3764,#2685,.T.) ;
#4654 = EDGE_CURVE('',#3765,#3764,#25,.T.) ;
#4655 = EDGE_CURVE('',#3662,#3765,#26,.T.) ;
#4656 = EDGE_CURVE('',#3764,#3661,#27,.T.) ;
#4657 = EDGE_CURVE('',#3765,#3766,#2686,.T.) ;
#4658 = EDGE_CURVE('',#3664,#3766,#28,.T.) ;
#4659 = EDGE_CURVE('',#3766,#3663,#29,.T.) ;
#4660 = EDGE_CURVE('',#3766,#3767,#2687,.T.) ;
#4661 = EDGE_CURVE('',#3768,#3767,#30,.T.) ;
#4662 = EDGE_CURVE('',#3666,#3768,#31,.T.) ;
#4663 = EDGE_CURVE('',#3767,#3665,#32,.T.) ;
#4664 = EDGE_CURVE('',#3768,#3769,#2688,.T.) ;
#4665 = EDGE_CURVE('',#3668,#3769,#33,.T.) ;
#4666 = EDGE_CURVE('',#3769,#3667,#34,.T.) ;
#4667 = EDGE_CURVE('',#3669,#3671,#2689,.T.) ;
#4668 = EDGE_CURVE('',#3672,#3670,#35,.T.) ;
#4669 = EDGE_CURVE('',#3673,#3675,#2690,.T.) ;
#4670 = EDGE_CURVE('',#3676,#3674,#36,.T.) ;
#4671 = EDGE_CURVE('',#3677,#3679,#2691,.T.) ;
#4672 = EDGE_CURVE('',#3680,#3678,#37,.T.) ;
#4673 = EDGE_CURVE('',#3681,#3683,#2692,.T.) ;
#4674 = EDGE_CURVE('',#3770,#3682,#38,.T.) ;
#4675 = EDGE_CURVE('',#3684,#3770,#39,.T.) ;
#4676 = EDGE_CURVE('',#3770,#3771,#2693,.T.) ;
#4677 = EDGE_CURVE('',#3772,#3771,#40,.T.) ;
#4678 = EDGE_CURVE('',#3686,#3772,#41,.T.) ;
#4679 = EDGE_CURVE('',#3771,#3685,#42,.T.) ;
#4680 = EDGE_CURVE('',#3772,#3773,#2694,.T.) ;
#4681 = EDGE_CURVE('',#3688,#3773,#43,.T.) ;
#4682 = EDGE_CURVE('',#3773,#3687,#44,.T.) ;
#4683 = EDGE_CURVE('',#3773,#3774,#2695,.T.) ;
#4684 = EDGE_CURVE('',#3775,#3774,#45,.T.) ;
#4685 = EDGE_CURVE('',#3690,#3775,#46,.T.) ;
#4686 = EDGE_CURVE('',#3774,#3689,#47,.T.) ;
#4687 = EDGE_CURVE('',#3775,#3776,#2696,.T.) ;
#4688 = EDGE_CURVE('',#3692,#3776,#48,.T.) ;
#4689 = EDGE_CURVE('',#3776,#3691,#49,.T.) ;
#4690 = EDGE_CURVE('',#3693,#3695,#2697,.T.) ;
#4691 = EDGE_CURVE('',#3696,#3694,#50,.T.) ;
#4692 = EDGE_CURVE('',#3697,#3699,#2698,.T.) ;
#4693 = EDGE_CURVE('',#3700,#3698,#51,.T.) ;
#4694 = EDGE_CURVE('',#3701,#3703,#2699,.T.) ;
#4695 = EDGE_CURVE('',#3704,#3702,#52,.T.) ;
#4696 = EDGE_CURVE('',#3705,#3707,#2700,.T.) ;
#4697 = EDGE_CURVE('',#3777,#3706,#53,.T.) ;
#4698 = EDGE_CURVE('',#3708,#3777,#54,.T.) ;
#4699 = EDGE_CURVE('',#3777,#3778,#2701,.T.) ;
#4700 = EDGE_CURVE('',#3779,#3778,#55,.T.) ;
#4701 = EDGE_CURVE('',#3710,#3779,#56,.T.) ;
#4702 = EDGE_CURVE('',#3778,#3709,#57,.T.) ;
#4703 = EDGE_CURVE('',#3779,#3780,#2702,.T.) ;
#4704 = EDGE_CURVE('',#3712,#3780,#58,.T.) ;
#4705 = EDGE_CURVE('',#3780,#3711,#59,.T.) ;
#4706 = EDGE_CURVE('',#3780,#3781,#2703,.T.) ;
#4707 = EDGE_CURVE('',#3782,#3781,#60,.T.) ;
#4708 = EDGE_CURVE('',#3714,#3782,#61,.T.) ;
#4709 = EDGE_CURVE('',#3781,#3713,#62,.T.) ;
#4710 = EDGE_CURVE('',#3782,#3783,#2704,.T.) ;
#4711 = EDGE_CURVE('',#3716,#3783,#63,.T.) ;
#4712 = EDGE_CURVE('',#3783,#3715,#64,.T.) ;
#4713 = EDGE_CURVE('',#3717,#3719,#2705,.T.) ;
#4714 = EDGE_CURVE('',#3720,#3718,#65,.T.) ;
#4715 = EDGE_CURVE('',#3721,#3723,#2706,.T.) ;
#4716 = EDGE_CURVE('',#3724,#3722,#66,.T.) ;
#4717 = EDGE_CURVE('',#3725,#3727,#2707,.T.) ;
#4718 = EDGE_CURVE('',#3728,#3726,#67,.T.) ;
#4719 = EDGE_CURVE('',#3729,#3731,#2708,.T.) ;
#4720 = EDGE_CURVE('',#3784,#3730,#68,.T.) ;
#4721 = EDGE_CURVE('',#3732,#3784,#69,.T.) ;
#4722 = EDGE_CURVE('',#3784,#3785,#2709,.T.) ;
#4723 = EDGE_CURVE('',#3786,#3785,#70,.T.) ;
#4724 = EDGE_CURVE('',#3734,#3786,#71,.T.) ;
#4725 = EDGE_CURVE('',#3785,#3733,#72,.T.) ;
#4726 = EDGE_CURVE('',#3786,#3787,#2710,.T.) ;
#4727 = EDGE_CURVE('',#3736,#3787,#73,.T.) ;
#4728 = EDGE_CURVE('',#3787,#3735,#74,.T.) ;
#4729 = EDGE_CURVE('',#3787,#3788,#2711,.T.) ;
#4730 = EDGE_CURVE('',#3789,#3788,#75,.T.) ;
#4731 = EDGE_CURVE('',#3738,#3789,#76,.T.) ;
#4732 = EDGE_CURVE('',#3788,#3737,#77,.T.) ;
#4733 = EDGE_CURVE('',#3789,#3790,#2712,.T.) ;
#4734 = EDGE_CURVE('',#3740,#3790,#78,.T.) ;
#4735 = EDGE_CURVE('',#3790,#3739,#79,.T.) ;
#4736 = EDGE_CURVE('',#3741,#3743,#2713,.T.) ;
#4737 = EDGE_CURVE('',#3744,#3742,#80,.T.) ;
#4738 = EDGE_CURVE('',#3745,#3747,#2714,.T.) ;
#4739 = EDGE_CURVE('',#3748,#3746,#81,.T.) ;
#4740 = EDGE_CURVE('',#3749,#3751,#2715,.T.) ;
#4741 = EDGE_CURVE('',#3752,#3750,#82,.T.) ;
#4742 = EDGE_CURVE('',#3753,#3755,#2716,.T.) ;
#4743 = EDGE_CURVE('',#3791,#3754,#83,.T.) ;
#4744 = EDGE_CURVE('',#3756,#3791,#84,.T.) ;
#4745 = EDGE_CURVE('',#3791,#3792,#2717,.T.) ;
#4746 = EDGE_CURVE('',#3793,#3792,#85,.T.) ;
#4747 = EDGE_CURVE('',#3758,#3793,#86,.T.) ;
#4748 = EDGE_CURVE('',#3792,#3757,#87,.T.) ;
#4749 = EDGE_CURVE('',#3793,#3794,#2718,.T.) ;
#4750 = EDGE_CURVE('',#3794,#3794,#1138,.T.) ;
#4751 = EDGE_CURVE('',#3795,#3795,#1139,.T.) ;
#4752 = EDGE_CURVE('',#3796,#3796,#1140,.T.) ;
#4753 = EDGE_CURVE('',#3797,#3797,#1141,.T.) ;
#4754 = EDGE_CURVE('',#3798,#3798,#1142,.T.) ;
#4755 = EDGE_CURVE('',#3797,#3795,#2719,.T.) ;
#4756 = EDGE_CURVE('',#3799,#3799,#1143,.T.) ;
#4757 = EDGE_CURVE('',#3799,#3798,#2720,.T.) ;
#4758 = EDGE_CURVE('',#3796,#3800,#2721,.T.) ;
#4759 = EDGE_CURVE('',#3800,#3800,#1144,.T.) ;
#4760 = EDGE_CURVE('',#3801,#3802,#2722,.T.) ;
#4761 = EDGE_CURVE('',#3802,#3803,#2723,.T.) ;
#4762 = EDGE_CURVE('',#3803,#3804,#2724,.T.) ;
#4763 = EDGE_CURVE('',#3804,#3801,#2725,.T.) ;
#4764 = EDGE_CURVE('',#3804,#3805,#2726,.T.) ;
#4765 = EDGE_CURVE('',#3806,#3805,#2727,.T.) ;
#4766 = EDGE_CURVE('',#3801,#3806,#2728,.T.) ;
#4767 = EDGE_CURVE('',#3803,#3807,#2729,.T.) ;
#4768 = EDGE_CURVE('',#3805,#3807,#2730,.T.) ;
#4769 = EDGE_CURVE('',#3802,#3808,#2731,.T.) ;
#4770 = EDGE_CURVE('',#3807,#3808,#2732,.T.) ;
#4771 = EDGE_CURVE('',#3808,#3806,#2733,.T.) ;
#4772 = EDGE_CURVE('',#3809,#3809,#1145,.T.) ;
#4773 = EDGE_CURVE('',#3809,#3810,#2734,.T.) ;
#4774 = EDGE_CURVE('',#3810,#3810,#1146,.T.) ;
#4775 = EDGE_CURVE('',#3811,#3812,#2735,.T.) ;
#4776 = EDGE_CURVE('',#3812,#3813,#2736,.T.) ;
#4777 = EDGE_CURVE('',#3813,#3814,#2737,.T.) ;
#4778 = EDGE_CURVE('',#3814,#3811,#2738,.T.) ;
#4779 = EDGE_CURVE('',#3815,#3816,#2739,.T.) ;
#4780 = EDGE_CURVE('',#3816,#3817,#2740,.T.) ;
#4781 = EDGE_CURVE('',#3817,#3818,#2741,.T.) ;
#4782 = EDGE_CURVE('',#3818,#3815,#2742,.T.) ;
#4783 = EDGE_CURVE('',#3814,#3817,#2743,.T.) ;
#4784 = EDGE_CURVE('',#3811,#3816,#2744,.T.) ;
#4785 = EDGE_CURVE('',#3813,#3818,#2745,.T.) ;
#4786 = EDGE_CURVE('',#3812,#3815,#2746,.T.) ;
#4787 = EDGE_CURVE('',#3819,#3820,#1147,.T.) ;
#4788 = EDGE_CURVE('',#3820,#3819,#1148,.T.) ;
#4789 = EDGE_CURVE('',#3821,#3822,#1149,.T.) ;
#4790 = EDGE_CURVE('',#3822,#3823,#1150,.T.) ;
#4791 = EDGE_CURVE('',#3823,#3821,#1151,.T.) ;
#4792 = EDGE_CURVE('',#3824,#3825,#1152,.T.) ;
#4793 = EDGE_CURVE('',#3825,#3826,#1153,.T.) ;
#4794 = EDGE_CURVE('',#3826,#3827,#1154,.T.) ;
#4795 = EDGE_CURVE('',#3827,#3824,#1155,.T.) ;
#4796 = EDGE_CURVE('',#3828,#3829,#1156,.T.) ;
#4797 = EDGE_CURVE('',#3829,#3830,#1157,.T.) ;
#4798 = EDGE_CURVE('',#3830,#3831,#1158,.T.) ;
#4799 = EDGE_CURVE('',#3831,#3828,#1159,.T.) ;
#4800 = EDGE_CURVE('',#3832,#3833,#1160,.T.) ;
#4801 = EDGE_CURVE('',#3833,#3834,#1161,.T.) ;
#4802 = EDGE_CURVE('',#3834,#3835,#1162,.T.) ;
#4803 = EDGE_CURVE('',#3835,#3832,#1163,.T.) ;
#4804 = EDGE_CURVE('',#3836,#3837,#1164,.T.) ;
#4805 = EDGE_CURVE('',#3837,#3838,#1165,.T.) ;
#4806 = EDGE_CURVE('',#3838,#3836,#1166,.T.) ;
#4807 = EDGE_CURVE('',#3839,#3840,#1167,.T.) ;
#4808 = EDGE_CURVE('',#3840,#3839,#1168,.T.) ;
#4809 = EDGE_CURVE('',#3841,#3842,#1169,.T.) ;
#4810 = EDGE_CURVE('',#3842,#3841,#1170,.T.) ;
#4811 = EDGE_CURVE('',#3843,#3844,#1171,.T.) ;
#4812 = EDGE_CURVE('',#3844,#3843,#1172,.T.) ;
#4813 = EDGE_CURVE('',#3845,#3846,#1173,.T.) ;
#4814 = EDGE_CURVE('',#3846,#3847,#1174,.T.) ;
#4815 = EDGE_CURVE('',#3847,#3845,#1175,.T.) ;
#4816 = EDGE_CURVE('',#3848,#3849,#1176,.T.) ;
#4817 = EDGE_CURVE('',#3849,#3850,#1177,.T.) ;
#4818 = EDGE_CURVE('',#3850,#3851,#1178,.T.) ;
#4819 = EDGE_CURVE('',#3851,#3848,#1179,.T.) ;
#4820 = EDGE_CURVE('',#3852,#3853,#1180,.T.) ;
#4821 = EDGE_CURVE('',#3853,#3854,#1181,.T.) ;
#4822 = EDGE_CURVE('',#3854,#3855,#1182,.T.) ;
#4823 = EDGE_CURVE('',#3855,#3852,#1183,.T.) ;
#4824 = EDGE_CURVE('',#3856,#3857,#1184,.T.) ;
#4825 = EDGE_CURVE('',#3857,#3858,#1185,.T.) ;
#4826 = EDGE_CURVE('',#3858,#3859,#1186,.T.) ;
#4827 = EDGE_CURVE('',#3859,#3856,#1187,.T.) ;
#4828 = EDGE_CURVE('',#3860,#3861,#1188,.T.) ;
#4829 = EDGE_CURVE('',#3861,#3862,#1189,.T.) ;
#4830 = EDGE_CURVE('',#3862,#3860,#1190,.T.) ;
#4831 = EDGE_CURVE('',#3863,#3864,#1191,.T.) ;
#4832 = EDGE_CURVE('',#3864,#3863,#1192,.T.) ;
#4833 = EDGE_CURVE('',#3865,#3866,#1193,.T.) ;
#4834 = EDGE_CURVE('',#3866,#3865,#1194,.T.) ;
#4835 = EDGE_CURVE('',#3867,#3868,#1195,.T.) ;
#4836 = EDGE_CURVE('',#3868,#3867,#1196,.T.) ;
#4837 = EDGE_CURVE('',#3869,#3870,#1197,.T.) ;
#4838 = EDGE_CURVE('',#3870,#3871,#1198,.T.) ;
#4839 = EDGE_CURVE('',#3871,#3869,#1199,.T.) ;
#4840 = EDGE_CURVE('',#3872,#3873,#1200,.T.) ;
#4841 = EDGE_CURVE('',#3873,#3874,#1201,.T.) ;
#4842 = EDGE_CURVE('',#3874,#3875,#1202,.T.) ;
#4843 = EDGE_CURVE('',#3875,#3872,#1203,.T.) ;
#4844 = EDGE_CURVE('',#3876,#3877,#1204,.T.) ;
#4845 = EDGE_CURVE('',#3877,#3878,#1205,.T.) ;
#4846 = EDGE_CURVE('',#3878,#3879,#1206,.T.) ;
#4847 = EDGE_CURVE('',#3879,#3876,#1207,.T.) ;
#4848 = EDGE_CURVE('',#3880,#3881,#1208,.T.) ;
#4849 = EDGE_CURVE('',#3881,#3882,#1209,.T.) ;
#4850 = EDGE_CURVE('',#3882,#3883,#1210,.T.) ;
#4851 = EDGE_CURVE('',#3883,#3880,#1211,.T.) ;
#4852 = EDGE_CURVE('',#3884,#3885,#1212,.T.) ;
#4853 = EDGE_CURVE('',#3885,#3886,#1213,.T.) ;
#4854 = EDGE_CURVE('',#3886,#3884,#1214,.T.) ;
#4855 = EDGE_CURVE('',#3887,#3888,#1215,.T.) ;
#4856 = EDGE_CURVE('',#3888,#3887,#1216,.T.) ;
#4857 = EDGE_CURVE('',#3889,#3889,#1217,.T.) ;
#4858 = EDGE_CURVE('',#3889,#3890,#2747,.T.) ;
#4859 = EDGE_CURVE('',#3891,#3890,#88,.T.) ;
#4860 = EDGE_CURVE('',#3820,#3891,#89,.T.) ;
#4861 = EDGE_CURVE('',#3890,#3819,#90,.T.) ;
#4862 = EDGE_CURVE('',#3891,#3892,#2748,.T.) ;
#4863 = EDGE_CURVE('',#3822,#3892,#91,.T.) ;
#4864 = EDGE_CURVE('',#3892,#3821,#92,.T.) ;
#4865 = EDGE_CURVE('',#3823,#3825,#2749,.T.) ;
#4866 = EDGE_CURVE('',#3826,#3824,#93,.T.) ;
#4867 = EDGE_CURVE('',#3827,#3829,#2750,.T.) ;
#4868 = EDGE_CURVE('',#3830,#3828,#94,.T.) ;
#4869 = EDGE_CURVE('',#3831,#3833,#2751,.T.) ;
#4870 = EDGE_CURVE('',#3834,#3832,#95,.T.) ;
#4871 = EDGE_CURVE('',#3835,#3837,#2752,.T.) ;
#4872 = EDGE_CURVE('',#3893,#3836,#96,.T.) ;
#4873 = EDGE_CURVE('',#3838,#3893,#97,.T.) ;
#4874 = EDGE_CURVE('',#3893,#3894,#2753,.T.) ;
#4875 = EDGE_CURVE('',#3895,#3894,#98,.T.) ;
#4876 = EDGE_CURVE('',#3840,#3895,#99,.T.) ;
#4877 = EDGE_CURVE('',#3894,#3839,#100,.T.) ;
#4878 = EDGE_CURVE('',#3895,#3896,#2754,.T.) ;
#4879 = EDGE_CURVE('',#3842,#3896,#101,.T.) ;
#4880 = EDGE_CURVE('',#3896,#3841,#102,.T.) ;
#4881 = EDGE_CURVE('',#3896,#3897,#2755,.T.) ;
#4882 = EDGE_CURVE('',#3898,#3897,#103,.T.) ;
#4883 = EDGE_CURVE('',#3844,#3898,#104,.T.) ;
#4884 = EDGE_CURVE('',#3897,#3843,#105,.T.) ;
#4885 = EDGE_CURVE('',#3898,#3899,#2756,.T.) ;
#4886 = EDGE_CURVE('',#3846,#3899,#106,.T.) ;
#4887 = EDGE_CURVE('',#3899,#3845,#107,.T.) ;
#4888 = EDGE_CURVE('',#3847,#3849,#2757,.T.) ;
#4889 = EDGE_CURVE('',#3850,#3848,#108,.T.) ;
#4890 = EDGE_CURVE('',#3851,#3853,#2758,.T.) ;
#4891 = EDGE_CURVE('',#3854,#3852,#109,.T.) ;
#4892 = EDGE_CURVE('',#3855,#3857,#2759,.T.) ;
#4893 = EDGE_CURVE('',#3858,#3856,#110,.T.) ;
#4894 = EDGE_CURVE('',#3859,#3861,#2760,.T.) ;
#4895 = EDGE_CURVE('',#3900,#3860,#111,.T.) ;
#4896 = EDGE_CURVE('',#3862,#3900,#112,.T.) ;
#4897 = EDGE_CURVE('',#3900,#3901,#2761,.T.) ;
#4898 = EDGE_CURVE('',#3902,#3901,#113,.T.) ;
#4899 = EDGE_CURVE('',#3864,#3902,#114,.T.) ;
#4900 = EDGE_CURVE('',#3901,#3863,#115,.T.) ;
#4901 = EDGE_CURVE('',#3902,#3903,#2762,.T.) ;
#4902 = EDGE_CURVE('',#3866,#3903,#116,.T.) ;
#4903 = EDGE_CURVE('',#3903,#3865,#117,.T.) ;
#4904 = EDGE_CURVE('',#3903,#3904,#2763,.T.) ;
#4905 = EDGE_CURVE('',#3905,#3904,#118,.T.) ;
#4906 = EDGE_CURVE('',#3868,#3905,#119,.T.) ;
#4907 = EDGE_CURVE('',#3904,#3867,#120,.T.) ;
#4908 = EDGE_CURVE('',#3905,#3906,#2764,.T.) ;
#4909 = EDGE_CURVE('',#3870,#3906,#121,.T.) ;
#4910 = EDGE_CURVE('',#3906,#3869,#122,.T.) ;
#4911 = EDGE_CURVE('',#3871,#3873,#2765,.T.) ;
#4912 = EDGE_CURVE('',#3874,#3872,#123,.T.) ;
#4913 = EDGE_CURVE('',#3875,#3877,#2766,.T.) ;
#4914 = EDGE_CURVE('',#3878,#3876,#124,.T.) ;
#4915 = EDGE_CURVE('',#3879,#3881,#2767,.T.) ;
#4916 = EDGE_CURVE('',#3882,#3880,#125,.T.) ;
#4917 = EDGE_CURVE('',#3883,#3885,#2768,.T.) ;
#4918 = EDGE_CURVE('',#3907,#3884,#126,.T.) ;
#4919 = EDGE_CURVE('',#3886,#3907,#127,.T.) ;
#4920 = EDGE_CURVE('',#3907,#3908,#2769,.T.) ;
#4921 = EDGE_CURVE('',#3909,#3908,#128,.T.) ;
#4922 = EDGE_CURVE('',#3888,#3909,#129,.T.) ;
#4923 = EDGE_CURVE('',#3908,#3887,#130,.T.) ;
#4924 = EDGE_CURVE('',#3909,#3910,#2770,.T.) ;
#4925 = EDGE_CURVE('',#3910,#3910,#1218,.T.) ;
#4926 = EDGE_CURVE('',#3911,#3911,#1219,.T.) ;
#4927 = EDGE_CURVE('',#3911,#3912,#2771,.T.) ;
#4928 = EDGE_CURVE('',#3912,#3912,#1220,.T.) ;
#4929 = EDGE_CURVE('',#3913,#3914,#2772,.T.) ;
#4930 = EDGE_CURVE('',#3914,#3915,#2773,.T.) ;
#4931 = EDGE_CURVE('',#3915,#3916,#2774,.T.) ;
#4932 = EDGE_CURVE('',#3916,#3913,#2775,.T.) ;
#4933 = EDGE_CURVE('',#3917,#3918,#2776,.T.) ;
#4934 = EDGE_CURVE('',#3918,#3919,#2777,.T.) ;
#4935 = EDGE_CURVE('',#3919,#3920,#2778,.T.) ;
#4936 = EDGE_CURVE('',#3920,#3917,#2779,.T.) ;
#4937 = EDGE_CURVE('',#3916,#3919,#2780,.T.) ;
#4938 = EDGE_CURVE('',#3913,#3918,#2781,.T.) ;
#4939 = EDGE_CURVE('',#3915,#3920,#2782,.T.) ;
#4940 = EDGE_CURVE('',#3914,#3917,#2783,.T.) ;
#4941 = EDGE_CURVE('',#3921,#3921,#1221,.T.) ;
#4942 = EDGE_CURVE('',#3921,#3922,#2784,.T.) ;
#4943 = EDGE_CURVE('',#3922,#3922,#1222,.T.) ;
#4944 = EDGE_CURVE('',#3923,#3923,#1223,.T.) ;
#4945 = EDGE_CURVE('',#3923,#3924,#2785,.T.) ;
#4946 = EDGE_CURVE('',#3924,#3924,#1224,.T.) ;
#4947 = EDGE_CURVE('',#3925,#3925,#1225,.T.) ;
#4948 = EDGE_CURVE('',#3925,#3926,#2786,.T.) ;
#4949 = EDGE_CURVE('',#3926,#3926,#1226,.T.) ;
#4950 = EDGE_CURVE('',#3927,#3927,#1227,.T.) ;
#4951 = EDGE_CURVE('',#3927,#3928,#2787,.T.) ;
#4952 = EDGE_CURVE('',#3928,#3928,#1228,.T.) ;
#4953 = EDGE_CURVE('',#3929,#3930,#1229,.T.) ;
#4954 = EDGE_CURVE('',#3930,#3929,#1230,.T.) ;
#4955 = EDGE_CURVE('',#3931,#3932,#1231,.T.) ;
#4956 = EDGE_CURVE('',#3932,#3933,#1232,.T.) ;
#4957 = EDGE_CURVE('',#3933,#3931,#1233,.T.) ;
#4958 = EDGE_CURVE('',#3934,#3935,#1234,.T.) ;
#4959 = EDGE_CURVE('',#3935,#3936,#1235,.T.) ;
#4960 = EDGE_CURVE('',#3936,#3937,#1236,.T.) ;
#4961 = EDGE_CURVE('',#3937,#3934,#1237,.T.) ;
#4962 = EDGE_CURVE('',#3938,#3939,#1238,.T.) ;
#4963 = EDGE_CURVE('',#3939,#3940,#1239,.T.) ;
#4964 = EDGE_CURVE('',#3940,#3941,#1240,.T.) ;
#4965 = EDGE_CURVE('',#3941,#3938,#1241,.T.) ;
#4966 = EDGE_CURVE('',#3942,#3943,#1242,.T.) ;
#4967 = EDGE_CURVE('',#3943,#3944,#1243,.T.) ;
#4968 = EDGE_CURVE('',#3944,#3945,#1244,.T.) ;
#4969 = EDGE_CURVE('',#3945,#3942,#1245,.T.) ;
#4970 = EDGE_CURVE('',#3946,#3947,#1246,.T.) ;
#4971 = EDGE_CURVE('',#3947,#3948,#1247,.T.) ;
#4972 = EDGE_CURVE('',#3948,#3946,#1248,.T.) ;
#4973 = EDGE_CURVE('',#3949,#3950,#1249,.T.) ;
#4974 = EDGE_CURVE('',#3950,#3949,#1250,.T.) ;
#4975 = EDGE_CURVE('',#3951,#3952,#1251,.T.) ;
#4976 = EDGE_CURVE('',#3952,#3951,#1252,.T.) ;
#4977 = EDGE_CURVE('',#3953,#3954,#1253,.T.) ;
#4978 = EDGE_CURVE('',#3954,#3953,#1254,.T.) ;
#4979 = EDGE_CURVE('',#3955,#3956,#1255,.T.) ;
#4980 = EDGE_CURVE('',#3956,#3957,#1256,.T.) ;
#4981 = EDGE_CURVE('',#3957,#3955,#1257,.T.) ;
#4982 = EDGE_CURVE('',#3958,#3959,#1258,.T.) ;
#4983 = EDGE_CURVE('',#3959,#3960,#1259,.T.) ;
#4984 = EDGE_CURVE('',#3960,#3961,#1260,.T.) ;
#4985 = EDGE_CURVE('',#3961,#3958,#1261,.T.) ;
#4986 = EDGE_CURVE('',#3962,#3963,#1262,.T.) ;
#4987 = EDGE_CURVE('',#3963,#3964,#1263,.T.) ;
#4988 = EDGE_CURVE('',#3964,#3965,#1264,.T.) ;
#4989 = EDGE_CURVE('',#3965,#3962,#1265,.T.) ;
#4990 = EDGE_CURVE('',#3966,#3967,#1266,.T.) ;
#4991 = EDGE_CURVE('',#3967,#3968,#1267,.T.) ;
#4992 = EDGE_CURVE('',#3968,#3969,#1268,.T.) ;
#4993 = EDGE_CURVE('',#3969,#3966,#1269,.T.) ;
#4994 = EDGE_CURVE('',#3970,#3971,#1270,.T.) ;
#4995 = EDGE_CURVE('',#3971,#3972,#1271,.T.) ;
#4996 = EDGE_CURVE('',#3972,#3970,#1272,.T.) ;
#4997 = EDGE_CURVE('',#3973,#3974,#1273,.T.) ;
#4998 = EDGE_CURVE('',#3974,#3973,#1274,.T.) ;
#4999 = EDGE_CURVE('',#3975,#3976,#1275,.T.) ;
#5000 = EDGE_CURVE('',#3976,#3975,#1276,.T.) ;
#5001 = EDGE_CURVE('',#3977,#3978,#1277,.T.) ;
#5002 = EDGE_CURVE('',#3978,#3977,#1278,.T.) ;
#5003 = EDGE_CURVE('',#3979,#3980,#1279,.T.) ;
#5004 = EDGE_CURVE('',#3980,#3981,#1280,.T.) ;
#5005 = EDGE_CURVE('',#3981,#3979,#1281,.T.) ;
#5006 = EDGE_CURVE('',#3982,#3983,#1282,.T.) ;
#5007 = EDGE_CURVE('',#3983,#3984,#1283,.T.) ;
#5008 = EDGE_CURVE('',#3984,#3985,#1284,.T.) ;
#5009 = EDGE_CURVE('',#3985,#3982,#1285,.T.) ;
#5010 = EDGE_CURVE('',#3986,#3987,#1286,.T.) ;
#5011 = EDGE_CURVE('',#3987,#3988,#1287,.T.) ;
#5012 = EDGE_CURVE('',#3988,#3989,#1288,.T.) ;
#5013 = EDGE_CURVE('',#3989,#3986,#1289,.T.) ;
#5014 = EDGE_CURVE('',#3990,#3991,#1290,.T.) ;
#5015 = EDGE_CURVE('',#3991,#3992,#1291,.T.) ;
#5016 = EDGE_CURVE('',#3992,#3993,#1292,.T.) ;
#5017 = EDGE_CURVE('',#3993,#3990,#1293,.T.) ;
#5018 = EDGE_CURVE('',#3994,#3995,#1294,.T.) ;
#5019 = EDGE_CURVE('',#3995,#3996,#1295,.T.) ;
#5020 = EDGE_CURVE('',#3996,#3994,#1296,.T.) ;
#5021 = EDGE_CURVE('',#3997,#3998,#1297,.T.) ;
#5022 = EDGE_CURVE('',#3998,#3997,#1298,.T.) ;
#5023 = EDGE_CURVE('',#3999,#4000,#1299,.T.) ;
#5024 = EDGE_CURVE('',#4000,#3999,#1300,.T.) ;
#5025 = EDGE_CURVE('',#4001,#4002,#1301,.T.) ;
#5026 = EDGE_CURVE('',#4002,#4001,#1302,.T.) ;
#5027 = EDGE_CURVE('',#4003,#4004,#1303,.T.) ;
#5028 = EDGE_CURVE('',#4004,#4005,#1304,.T.) ;
#5029 = EDGE_CURVE('',#4005,#4003,#1305,.T.) ;
#5030 = EDGE_CURVE('',#4006,#4007,#1306,.T.) ;
#5031 = EDGE_CURVE('',#4007,#4008,#1307,.T.) ;
#5032 = EDGE_CURVE('',#4008,#4009,#1308,.T.) ;
#5033 = EDGE_CURVE('',#4009,#4006,#1309,.T.) ;
#5034 = EDGE_CURVE('',#4010,#4011,#1310,.T.) ;
#5035 = EDGE_CURVE('',#4011,#4012,#1311,.T.) ;
#5036 = EDGE_CURVE('',#4012,#4013,#1312,.T.) ;
#5037 = EDGE_CURVE('',#4013,#4010,#1313,.T.) ;
#5038 = EDGE_CURVE('',#4014,#4015,#1314,.T.) ;
#5039 = EDGE_CURVE('',#4015,#4016,#1315,.T.) ;
#5040 = EDGE_CURVE('',#4016,#4017,#1316,.T.) ;
#5041 = EDGE_CURVE('',#4017,#4014,#1317,.T.) ;
#5042 = EDGE_CURVE('',#4018,#4019,#1318,.T.) ;
#5043 = EDGE_CURVE('',#4019,#4020,#1319,.T.) ;
#5044 = EDGE_CURVE('',#4020,#4018,#1320,.T.) ;
#5045 = EDGE_CURVE('',#4021,#4022,#1321,.T.) ;
#5046 = EDGE_CURVE('',#4022,#4021,#1322,.T.) ;
#5047 = EDGE_CURVE('',#4023,#4023,#1323,.T.) ;
#5048 = EDGE_CURVE('',#4023,#4024,#2788,.T.) ;
#5049 = EDGE_CURVE('',#4025,#4024,#131,.T.) ;
#5050 = EDGE_CURVE('',#3930,#4025,#132,.T.) ;
#5051 = EDGE_CURVE('',#4024,#3929,#133,.T.) ;
#5052 = EDGE_CURVE('',#4025,#4026,#2789,.T.) ;
#5053 = EDGE_CURVE('',#3932,#4026,#134,.T.) ;
#5054 = EDGE_CURVE('',#4026,#3931,#135,.T.) ;
#5055 = EDGE_CURVE('',#3933,#3935,#2790,.T.) ;
#5056 = EDGE_CURVE('',#3936,#3934,#136,.T.) ;
#5057 = EDGE_CURVE('',#3937,#3939,#2791,.T.) ;
#5058 = EDGE_CURVE('',#3940,#3938,#137,.T.) ;
#5059 = EDGE_CURVE('',#3941,#3943,#2792,.T.) ;
#5060 = EDGE_CURVE('',#3944,#3942,#138,.T.) ;
#5061 = EDGE_CURVE('',#3945,#3947,#2793,.T.) ;
#5062 = EDGE_CURVE('',#4027,#3946,#139,.T.) ;
#5063 = EDGE_CURVE('',#3948,#4027,#140,.T.) ;
#5064 = EDGE_CURVE('',#4027,#4028,#2794,.T.) ;
#5065 = EDGE_CURVE('',#4029,#4028,#141,.T.) ;
#5066 = EDGE_CURVE('',#3950,#4029,#142,.T.) ;
#5067 = EDGE_CURVE('',#4028,#3949,#143,.T.) ;
#5068 = EDGE_CURVE('',#4029,#4030,#2795,.T.) ;
#5069 = EDGE_CURVE('',#3952,#4030,#144,.T.) ;
#5070 = EDGE_CURVE('',#4030,#3951,#145,.T.) ;
#5071 = EDGE_CURVE('',#4030,#4031,#2796,.T.) ;
#5072 = EDGE_CURVE('',#4032,#4031,#146,.T.) ;
#5073 = EDGE_CURVE('',#3954,#4032,#147,.T.) ;
#5074 = EDGE_CURVE('',#4031,#3953,#148,.T.) ;
#5075 = EDGE_CURVE('',#4032,#4033,#2797,.T.) ;
#5076 = EDGE_CURVE('',#3956,#4033,#149,.T.) ;
#5077 = EDGE_CURVE('',#4033,#3955,#150,.T.) ;
#5078 = EDGE_CURVE('',#3957,#3959,#2798,.T.) ;
#5079 = EDGE_CURVE('',#3960,#3958,#151,.T.) ;
#5080 = EDGE_CURVE('',#3961,#3963,#2799,.T.) ;
#5081 = EDGE_CURVE('',#3964,#3962,#152,.T.) ;
#5082 = EDGE_CURVE('',#3965,#3967,#2800,.T.) ;
#5083 = EDGE_CURVE('',#3968,#3966,#153,.T.) ;
#5084 = EDGE_CURVE('',#3969,#3971,#2801,.T.) ;
#5085 = EDGE_CURVE('',#4034,#3970,#154,.T.) ;
#5086 = EDGE_CURVE('',#3972,#4034,#155,.T.) ;
#5087 = EDGE_CURVE('',#4034,#4035,#2802,.T.) ;
#5088 = EDGE_CURVE('',#4036,#4035,#156,.T.) ;
#5089 = EDGE_CURVE('',#3974,#4036,#157,.T.) ;
#5090 = EDGE_CURVE('',#4035,#3973,#158,.T.) ;
#5091 = EDGE_CURVE('',#4036,#4037,#2803,.T.) ;
#5092 = EDGE_CURVE('',#3976,#4037,#159,.T.) ;
#5093 = EDGE_CURVE('',#4037,#3975,#160,.T.) ;
#5094 = EDGE_CURVE('',#4037,#4038,#2804,.T.) ;
#5095 = EDGE_CURVE('',#4039,#4038,#161,.T.) ;
#5096 = EDGE_CURVE('',#3978,#4039,#162,.T.) ;
#5097 = EDGE_CURVE('',#4038,#3977,#163,.T.) ;
#5098 = EDGE_CURVE('',#4039,#4040,#2805,.T.) ;
#5099 = EDGE_CURVE('',#3980,#4040,#164,.T.) ;
#5100 = EDGE_CURVE('',#4040,#3979,#165,.T.) ;
#5101 = EDGE_CURVE('',#3981,#3983,#2806,.T.) ;
#5102 = EDGE_CURVE('',#3984,#3982,#166,.T.) ;
#5103 = EDGE_CURVE('',#3985,#3987,#2807,.T.) ;
#5104 = EDGE_CURVE('',#3988,#3986,#167,.T.) ;
#5105 = EDGE_CURVE('',#3989,#3991,#2808,.T.) ;
#5106 = EDGE_CURVE('',#3992,#3990,#168,.T.) ;
#5107 = EDGE_CURVE('',#3993,#3995,#2809,.T.) ;
#5108 = EDGE_CURVE('',#4041,#3994,#169,.T.) ;
#5109 = EDGE_CURVE('',#3996,#4041,#170,.T.) ;
#5110 = EDGE_CURVE('',#4041,#4042,#2810,.T.) ;
#5111 = EDGE_CURVE('',#4043,#4042,#171,.T.) ;
#5112 = EDGE_CURVE('',#3998,#4043,#172,.T.) ;
#5113 = EDGE_CURVE('',#4042,#3997,#173,.T.) ;
#5114 = EDGE_CURVE('',#4043,#4044,#2811,.T.) ;
#5115 = EDGE_CURVE('',#4000,#4044,#174,.T.) ;
#5116 = EDGE_CURVE('',#4044,#3999,#175,.T.) ;
#5117 = EDGE_CURVE('',#4044,#4045,#2812,.T.) ;
#5118 = EDGE_CURVE('',#4046,#4045,#176,.T.) ;
#5119 = EDGE_CURVE('',#4002,#4046,#177,.T.) ;
#5120 = EDGE_CURVE('',#4045,#4001,#178,.T.) ;
#5121 = EDGE_CURVE('',#4046,#4047,#2813,.T.) ;
#5122 = EDGE_CURVE('',#4004,#4047,#179,.T.) ;
#5123 = EDGE_CURVE('',#4047,#4003,#180,.T.) ;
#5124 = EDGE_CURVE('',#4005,#4007,#2814,.T.) ;
#5125 = EDGE_CURVE('',#4008,#4006,#181,.T.) ;
#5126 = EDGE_CURVE('',#4009,#4011,#2815,.T.) ;
#5127 = EDGE_CURVE('',#4012,#4010,#182,.T.) ;
#5128 = EDGE_CURVE('',#4013,#4015,#2816,.T.) ;
#5129 = EDGE_CURVE('',#4016,#4014,#183,.T.) ;
#5130 = EDGE_CURVE('',#4017,#4019,#2817,.T.) ;
#5131 = EDGE_CURVE('',#4048,#4018,#184,.T.) ;
#5132 = EDGE_CURVE('',#4020,#4048,#185,.T.) ;
#5133 = EDGE_CURVE('',#4048,#4049,#2818,.T.) ;
#5134 = EDGE_CURVE('',#4050,#4049,#186,.T.) ;
#5135 = EDGE_CURVE('',#4022,#4050,#187,.T.) ;
#5136 = EDGE_CURVE('',#4049,#4021,#188,.T.) ;
#5137 = EDGE_CURVE('',#4050,#4051,#2819,.T.) ;
#5138 = EDGE_CURVE('',#4051,#4051,#1324,.T.) ;
#5139 = EDGE_CURVE('',#4052,#4052,#1325,.T.) ;
#5140 = EDGE_CURVE('',#4052,#4053,#2820,.T.) ;
#5141 = EDGE_CURVE('',#4053,#4053,#1326,.T.) ;
#5142 = EDGE_CURVE('',#4054,#4055,#2821,.T.) ;
#5143 = EDGE_CURVE('',#4056,#4054,#2822,.T.) ;
#5144 = EDGE_CURVE('',#4057,#4056,#2823,.T.) ;
#5145 = EDGE_CURVE('',#4057,#4055,#2824,.T.) ;
#5146 = EDGE_CURVE('',#4058,#4059,#2825,.T.) ;
#5147 = EDGE_CURVE('',#4059,#4057,#2826,.T.) ;
#5148 = EDGE_CURVE('',#4056,#4058,#2827,.T.) ;
#5149 = EDGE_CURVE('',#4060,#4061,#2828,.T.) ;
#5150 = EDGE_CURVE('',#4059,#4060,#2829,.T.) ;
#5151 = EDGE_CURVE('',#4058,#4061,#2830,.T.) ;
#5152 = EDGE_CURVE('',#4062,#4063,#2831,.T.) ;
#5153 = EDGE_CURVE('',#4063,#4064,#2832,.T.) ;
#5154 = EDGE_CURVE('',#4064,#4065,#2833,.T.) ;
#5155 = EDGE_CURVE('',#4065,#4062,#2834,.T.) ;
#5156 = EDGE_CURVE('',#4061,#4066,#2835,.T.) ;
#5157 = EDGE_CURVE('',#4066,#4067,#2836,.T.) ;
#5158 = EDGE_CURVE('',#4067,#4060,#2837,.T.) ;
#5159 = EDGE_CURVE('',#4055,#4068,#2838,.T.) ;
#5160 = EDGE_CURVE('',#4068,#4069,#2839,.T.) ;
#5161 = EDGE_CURVE('',#4069,#4054,#2840,.T.) ;
#5162 = EDGE_CURVE('',#4066,#4064,#2841,.T.) ;
#5163 = EDGE_CURVE('',#4069,#4065,#2842,.T.) ;
#5164 = EDGE_CURVE('',#4068,#4062,#2843,.T.) ;
#5165 = EDGE_CURVE('',#4067,#4063,#2844,.T.) ;
#5166 = EDGE_CURVE('',#4070,#4071,#2845,.T.) ;
#5167 = EDGE_CURVE('',#4072,#4070,#2846,.T.) ;
#5168 = EDGE_CURVE('',#4073,#4072,#2847,.T.) ;
#5169 = EDGE_CURVE('',#4071,#4073,#2848,.T.) ;
#5170 = EDGE_CURVE('',#4071,#4074,#2849,.T.) ;
#5171 = EDGE_CURVE('',#4073,#4075,#2850,.T.) ;
#5172 = EDGE_CURVE('',#4075,#4074,#2851,.T.) ;
#5173 = EDGE_CURVE('',#4074,#4076,#2852,.T.) ;
#5174 = EDGE_CURVE('',#4077,#4075,#2853,.T.) ;
#5175 = EDGE_CURVE('',#4076,#4077,#2854,.T.) ;
#5176 = EDGE_CURVE('',#4076,#4070,#2855,.T.) ;
#5177 = EDGE_CURVE('',#4072,#4077,#2856,.T.) ;
#5178 = EDGE_CURVE('',#4078,#4078,#1327,.T.) ;
#5179 = EDGE_CURVE('',#4078,#4079,#2857,.T.) ;
#5180 = EDGE_CURVE('',#4079,#4079,#1328,.T.) ;
#5181 = EDGE_CURVE('',#4080,#4081,#2858,.T.) ;
#5182 = EDGE_CURVE('',#4081,#4082,#2859,.T.) ;
#5183 = EDGE_CURVE('',#4082,#4083,#2860,.T.) ;
#5184 = EDGE_CURVE('',#4083,#4080,#2861,.T.) ;
#5185 = EDGE_CURVE('',#4084,#4085,#2862,.T.) ;
#5186 = EDGE_CURVE('',#4085,#4086,#2863,.T.) ;
#5187 = EDGE_CURVE('',#4086,#4087,#2864,.T.) ;
#5188 = EDGE_CURVE('',#4087,#4084,#2865,.T.) ;
#5189 = EDGE_CURVE('',#4083,#4086,#2866,.T.) ;
#5190 = EDGE_CURVE('',#4080,#4085,#2867,.T.) ;
#5191 = EDGE_CURVE('',#4082,#4087,#2868,.T.) ;
#5192 = EDGE_CURVE('',#4081,#4084,#2869,.T.) ;
#5193 = EDGE_CURVE('',#4088,#4089,#1329,.T.) ;
#5194 = EDGE_CURVE('',#4088,#4089,#1330,.T.) ;
#5195 = EDGE_CURVE('',#4089,#4088,#1331,.T.) ;
#5196 = EDGE_CURVE('',#4090,#4090,#1332,.T.) ;
#5197 = EDGE_CURVE('',#4090,#4088,#2870,.T.) ;
#5198 = EDGE_CURVE('',#4091,#4091,#1333,.T.) ;
#5199 = EDGE_CURVE('',#4091,#4092,#2871,.T.) ;
#5200 = EDGE_CURVE('',#4092,#4092,#1334,.T.) ;
#5201 = EDGE_CURVE('',#4093,#4093,#1335,.T.) ;
#5202 = EDGE_CURVE('',#4093,#4094,#2872,.T.) ;
#5203 = EDGE_CURVE('',#4094,#4094,#1336,.T.) ;
#5204 = EDGE_CURVE('',#4095,#4095,#1337,.T.) ;
#5205 = EDGE_CURVE('',#4095,#4096,#2873,.T.) ;
#5206 = EDGE_CURVE('',#4096,#4096,#1338,.T.) ;
#5207 = EDGE_CURVE('',#4097,#4097,#1339,.T.) ;
#5208 = EDGE_CURVE('',#4097,#4098,#2874,.T.) ;
#5209 = EDGE_CURVE('',#4098,#4098,#1340,.T.) ;
#5210 = EDGE_CURVE('',#4099,#4099,#1341,.T.) ;
#5211 = EDGE_CURVE('',#4099,#4100,#2875,.T.) ;
#5212 = EDGE_CURVE('',#4100,#4100,#1342,.T.) ;
#5213 = EDGE_CURVE('',#4101,#4102,#1343,.T.) ;
#5214 = EDGE_CURVE('',#4101,#4103,#2876,.T.) ;
#5215 = EDGE_CURVE('',#4104,#4103,#2877,.T.) ;
#5216 = EDGE_CURVE('',#4105,#4104,#2878,.T.) ;
#5217 = EDGE_CURVE('',#4106,#4105,#2879,.T.) ;
#5218 = EDGE_CURVE('',#4106,#4107,#2880,.T.) ;
#5219 = EDGE_CURVE('',#4102,#4107,#1344,.T.) ;
#5220 = EDGE_CURVE('',#4107,#4108,#2881,.T.) ;
#5221 = EDGE_CURVE('',#4109,#4106,#2882,.T.) ;
#5222 = EDGE_CURVE('',#4108,#4109,#2883,.T.) ;
#5223 = EDGE_CURVE('',#4110,#4101,#2884,.T.) ;
#5224 = EDGE_CURVE('',#4111,#4110,#2885,.T.) ;
#5225 = EDGE_CURVE('',#4103,#4111,#2886,.T.) ;
#5226 = EDGE_CURVE('',#4108,#4112,#1345,.T.) ;
#5227 = EDGE_CURVE('',#4113,#4109,#2887,.T.) ;
#5228 = EDGE_CURVE('',#4114,#4113,#2888,.T.) ;
#5229 = EDGE_CURVE('',#4111,#4114,#2889,.T.) ;
#5230 = EDGE_CURVE('',#4112,#4110,#1346,.T.) ;
#5231 = EDGE_CURVE('',#4115,#4114,#2890,.T.) ;
#5232 = EDGE_CURVE('',#4115,#4116,#2891,.T.) ;
#5233 = EDGE_CURVE('',#4117,#4116,#2892,.T.) ;
#5234 = EDGE_CURVE('',#4118,#4117,#2893,.T.) ;
#5235 = EDGE_CURVE('',#4104,#4118,#2894,.T.) ;
#5236 = EDGE_CURVE('',#4113,#4119,#2895,.T.) ;
#5237 = EDGE_CURVE('',#4119,#4115,#2896,.T.) ;
#5238 = EDGE_CURVE('',#4118,#4120,#2897,.T.) ;
#5239 = EDGE_CURVE('',#4120,#4105,#2898,.T.) ;
#5240 = EDGE_CURVE('',#4121,#4121,#1347,.T.) ;
#5241 = EDGE_CURVE('',#4121,#4102,#2899,.T.) ;
#5242 = EDGE_CURVE('',#4112,#4122,#2900,.T.) ;
#5243 = EDGE_CURVE('',#4122,#4122,#1348,.T.) ;
#5244 = EDGE_CURVE('',#4116,#4123,#2901,.T.) ;
#5245 = EDGE_CURVE('',#4123,#4124,#2902,.T.) ;
#5246 = EDGE_CURVE('',#4124,#4117,#2903,.T.) ;
#5247 = EDGE_CURVE('',#4120,#4124,#2904,.T.) ;
#5248 = EDGE_CURVE('',#4119,#4123,#2905,.T.) ;
#5249 = EDGE_CURVE('',#4125,#4125,#1349,.T.) ;
#5250 = EDGE_CURVE('',#4125,#4126,#2906,.T.) ;
#5251 = EDGE_CURVE('',#4126,#4126,#1350,.T.) ;
#5252 = EDGE_CURVE('',#4127,#4127,#1351,.T.) ;
#5253 = EDGE_CURVE('',#4127,#4128,#2907,.T.) ;
#5254 = EDGE_CURVE('',#4128,#4128,#1352,.T.) ;
#5255 = EDGE_CURVE('',#4129,#4129,#1353,.T.) ;
#5256 = EDGE_CURVE('',#4129,#4130,#2908,.T.) ;
#5257 = EDGE_CURVE('',#4130,#4130,#1354,.T.) ;
#5258 = EDGE_CURVE('',#4131,#4131,#1355,.T.) ;
#5259 = EDGE_CURVE('',#4131,#4132,#2909,.T.) ;
#5260 = EDGE_CURVE('',#4132,#4132,#1356,.T.) ;
#5261 = EDGE_CURVE('',#4133,#4133,#1357,.T.) ;
#5262 = EDGE_CURVE('',#4133,#4134,#2910,.T.) ;
#5263 = EDGE_CURVE('',#4134,#4134,#1358,.T.) ;
#5264 = EDGE_CURVE('',#4135,#4135,#1359,.T.) ;
#5265 = EDGE_CURVE('',#4135,#4136,#2911,.T.) ;
#5266 = EDGE_CURVE('',#4136,#4136,#1360,.T.) ;
#5267 = EDGE_CURVE('',#4137,#4137,#1361,.T.) ;
#5268 = EDGE_CURVE('',#4137,#4138,#2912,.T.) ;
#5269 = EDGE_CURVE('',#4138,#4138,#1362,.T.) ;
#5270 = EDGE_CURVE('',#4139,#4139,#1363,.T.) ;
#5271 = EDGE_CURVE('',#4139,#4140,#2913,.T.) ;
#5272 = EDGE_CURVE('',#4140,#4140,#1364,.T.) ;
#5273 = ORIENTED_EDGE('',*,*,#4141,.F.) ;
#5274 = ORIENTED_EDGE('',*,*,#4142,.F.) ;
#5275 = ORIENTED_EDGE('',*,*,#4143,.F.) ;
#5276 = ORIENTED_EDGE('',*,*,#4144,.F.) ;
#5277 = ORIENTED_EDGE('',*,*,#4144,.T.) ;
#5278 = ORIENTED_EDGE('',*,*,#4145,.F.) ;
#5279 = ORIENTED_EDGE('',*,*,#4146,.F.) ;
#5280 = ORIENTED_EDGE('',*,*,#4147,.T.) ;
#5281 = ORIENTED_EDGE('',*,*,#4148,.T.) ;
#5282 = ORIENTED_EDGE('',*,*,#4149,.T.) ;
#5283 = ORIENTED_EDGE('',*,*,#4143,.T.) ;
#5284 = ORIENTED_EDGE('',*,*,#4150,.F.) ;
#5285 = ORIENTED_EDGE('',*,*,#4151,.T.) ;
#5286 = ORIENTED_EDGE('',*,*,#4152,.F.) ;
#5287 = ORIENTED_EDGE('',*,*,#4153,.F.) ;
#5288 = ORIENTED_EDGE('',*,*,#4145,.T.) ;
#5289 = ORIENTED_EDGE('',*,*,#4142,.T.) ;
#5290 = ORIENTED_EDGE('',*,*,#4154,.F.) ;
#5291 = ORIENTED_EDGE('',*,*,#4155,.F.) ;
#5292 = ORIENTED_EDGE('',*,*,#4150,.T.) ;
#5293 = ORIENTED_EDGE('',*,*,#4141,.T.) ;
#5294 = ORIENTED_EDGE('',*,*,#4149,.F.) ;
#5295 = ORIENTED_EDGE('',*,*,#4156,.F.) ;
#5296 = ORIENTED_EDGE('',*,*,#4154,.T.) ;
#5297 = ORIENTED_EDGE('',*,*,#4155,.T.) ;
#5298 = ORIENTED_EDGE('',*,*,#4156,.T.) ;
#5299 = ORIENTED_EDGE('',*,*,#4148,.F.) ;
#5300 = ORIENTED_EDGE('',*,*,#4157,.F.) ;
#5301 = ORIENTED_EDGE('',*,*,#4158,.F.) ;
#5302 = ORIENTED_EDGE('',*,*,#4151,.F.) ;
#5303 = ORIENTED_EDGE('',*,*,#4159,.T.) ;
#5304 = ORIENTED_EDGE('',*,*,#4160,.T.) ;
#5305 = ORIENTED_EDGE('',*,*,#4161,.T.) ;
#5306 = ORIENTED_EDGE('',*,*,#4162,.T.) ;
#5307 = ORIENTED_EDGE('',*,*,#4163,.T.) ;
#5308 = ORIENTED_EDGE('',*,*,#4164,.T.) ;
#5309 = ORIENTED_EDGE('',*,*,#4165,.T.) ;
#5310 = ORIENTED_EDGE('',*,*,#4166,.T.) ;
#5311 = ORIENTED_EDGE('',*,*,#4167,.T.) ;
#5312 = ORIENTED_EDGE('',*,*,#4168,.T.) ;
#5313 = ORIENTED_EDGE('',*,*,#4169,.T.) ;
#5314 = ORIENTED_EDGE('',*,*,#4170,.T.) ;
#5315 = ORIENTED_EDGE('',*,*,#4171,.F.) ;
#5316 = ORIENTED_EDGE('',*,*,#4172,.T.) ;
#5317 = ORIENTED_EDGE('',*,*,#4173,.T.) ;
#5318 = ORIENTED_EDGE('',*,*,#4172,.F.) ;
#5319 = ORIENTED_EDGE('',*,*,#4173,.F.) ;
#5320 = ORIENTED_EDGE('',*,*,#4174,.F.) ;
#5321 = ORIENTED_EDGE('',*,*,#4175,.T.) ;
#5322 = ORIENTED_EDGE('',*,*,#4176,.T.) ;
#5323 = ORIENTED_EDGE('',*,*,#4175,.F.) ;
#5324 = ORIENTED_EDGE('',*,*,#4176,.F.) ;
#5325 = ORIENTED_EDGE('',*,*,#4177,.F.) ;
#5326 = ORIENTED_EDGE('',*,*,#4178,.T.) ;
#5327 = ORIENTED_EDGE('',*,*,#4179,.F.) ;
#5328 = ORIENTED_EDGE('',*,*,#4178,.F.) ;
#5329 = ORIENTED_EDGE('',*,*,#4180,.T.) ;
#5330 = ORIENTED_EDGE('',*,*,#4181,.F.) ;
#5331 = ORIENTED_EDGE('',*,*,#4182,.T.) ;
#5332 = ORIENTED_EDGE('',*,*,#4183,.T.) ;
#5333 = ORIENTED_EDGE('',*,*,#4179,.T.) ;
#5334 = ORIENTED_EDGE('',*,*,#4184,.T.) ;
#5335 = ORIENTED_EDGE('',*,*,#4185,.F.) ;
#5336 = ORIENTED_EDGE('',*,*,#4186,.F.) ;
#5337 = ORIENTED_EDGE('',*,*,#4183,.F.) ;
#5338 = ORIENTED_EDGE('',*,*,#4187,.F.) ;
#5339 = ORIENTED_EDGE('',*,*,#4188,.F.) ;
#5340 = ORIENTED_EDGE('',*,*,#4184,.F.) ;
#5341 = ORIENTED_EDGE('',*,*,#4182,.F.) ;
#5342 = ORIENTED_EDGE('',*,*,#4186,.T.) ;
#5343 = ORIENTED_EDGE('',*,*,#4189,.F.) ;
#5344 = ORIENTED_EDGE('',*,*,#4190,.F.) ;
#5345 = ORIENTED_EDGE('',*,*,#4180,.F.) ;
#5346 = ORIENTED_EDGE('',*,*,#4187,.T.) ;
#5347 = ORIENTED_EDGE('',*,*,#4181,.T.) ;
#5348 = ORIENTED_EDGE('',*,*,#4190,.T.) ;
#5349 = ORIENTED_EDGE('',*,*,#4191,.F.) ;
#5350 = ORIENTED_EDGE('',*,*,#4192,.F.) ;
#5351 = ORIENTED_EDGE('',*,*,#4193,.F.) ;
#5352 = ORIENTED_EDGE('',*,*,#4194,.T.) ;
#5353 = ORIENTED_EDGE('',*,*,#4195,.F.) ;
#5354 = ORIENTED_EDGE('',*,*,#4196,.F.) ;
#5355 = ORIENTED_EDGE('',*,*,#4197,.T.) ;
#5356 = ORIENTED_EDGE('',*,*,#4198,.F.) ;
#5357 = ORIENTED_EDGE('',*,*,#4197,.F.) ;
#5358 = ORIENTED_EDGE('',*,*,#4199,.T.) ;
#5359 = ORIENTED_EDGE('',*,*,#4200,.T.) ;
#5360 = ORIENTED_EDGE('',*,*,#4201,.T.) ;
#5361 = ORIENTED_EDGE('',*,*,#4202,.F.) ;
#5362 = ORIENTED_EDGE('',*,*,#4198,.T.) ;
#5363 = ORIENTED_EDGE('',*,*,#4203,.T.) ;
#5364 = ORIENTED_EDGE('',*,*,#4204,.F.) ;
#5365 = ORIENTED_EDGE('',*,*,#4205,.F.) ;
#5366 = ORIENTED_EDGE('',*,*,#4201,.F.) ;
#5367 = ORIENTED_EDGE('',*,*,#4206,.T.) ;
#5368 = ORIENTED_EDGE('',*,*,#4207,.F.) ;
#5369 = ORIENTED_EDGE('',*,*,#4203,.F.) ;
#5370 = ORIENTED_EDGE('',*,*,#4200,.F.) ;
#5371 = ORIENTED_EDGE('',*,*,#4208,.F.) ;
#5372 = ORIENTED_EDGE('',*,*,#4209,.F.) ;
#5373 = ORIENTED_EDGE('',*,*,#4206,.F.) ;
#5374 = ORIENTED_EDGE('',*,*,#4199,.F.) ;
#5375 = ORIENTED_EDGE('',*,*,#4208,.T.) ;
#5376 = ORIENTED_EDGE('',*,*,#4202,.T.) ;
#5377 = ORIENTED_EDGE('',*,*,#4205,.T.) ;
#5378 = ORIENTED_EDGE('',*,*,#4210,.F.) ;
#5379 = ORIENTED_EDGE('',*,*,#4211,.F.) ;
#5380 = ORIENTED_EDGE('',*,*,#4212,.F.) ;
#5381 = ORIENTED_EDGE('',*,*,#4213,.T.) ;
#5382 = ORIENTED_EDGE('',*,*,#4214,.F.) ;
#5383 = ORIENTED_EDGE('',*,*,#4215,.F.) ;
#5384 = ORIENTED_EDGE('',*,*,#4216,.T.) ;
#5385 = ORIENTED_EDGE('',*,*,#4217,.F.) ;
#5386 = ORIENTED_EDGE('',*,*,#4216,.F.) ;
#5387 = ORIENTED_EDGE('',*,*,#4218,.F.) ;
#5388 = ORIENTED_EDGE('',*,*,#4219,.T.) ;
#5389 = ORIENTED_EDGE('',*,*,#4159,.F.) ;
#5390 = ORIENTED_EDGE('',*,*,#4219,.F.) ;
#5391 = ORIENTED_EDGE('',*,*,#4218,.T.) ;
#5392 = ORIENTED_EDGE('',*,*,#4217,.T.) ;
#5393 = ORIENTED_EDGE('',*,*,#4215,.T.) ;
#5394 = ORIENTED_EDGE('',*,*,#4220,.F.) ;
#5395 = ORIENTED_EDGE('',*,*,#4221,.T.) ;
#5396 = ORIENTED_EDGE('',*,*,#4222,.F.) ;
#5397 = ORIENTED_EDGE('',*,*,#4221,.F.) ;
#5398 = ORIENTED_EDGE('',*,*,#4223,.F.) ;
#5399 = ORIENTED_EDGE('',*,*,#4224,.T.) ;
#5400 = ORIENTED_EDGE('',*,*,#4170,.F.) ;
#5401 = ORIENTED_EDGE('',*,*,#4224,.F.) ;
#5402 = ORIENTED_EDGE('',*,*,#4223,.T.) ;
#5403 = ORIENTED_EDGE('',*,*,#4222,.T.) ;
#5404 = ORIENTED_EDGE('',*,*,#4225,.F.) ;
#5405 = ORIENTED_EDGE('',*,*,#4226,.T.) ;
#5406 = ORIENTED_EDGE('',*,*,#4227,.F.) ;
#5407 = ORIENTED_EDGE('',*,*,#4226,.F.) ;
#5408 = ORIENTED_EDGE('',*,*,#4228,.F.) ;
#5409 = ORIENTED_EDGE('',*,*,#4229,.T.) ;
#5410 = ORIENTED_EDGE('',*,*,#4160,.F.) ;
#5411 = ORIENTED_EDGE('',*,*,#4229,.F.) ;
#5412 = ORIENTED_EDGE('',*,*,#4228,.T.) ;
#5413 = ORIENTED_EDGE('',*,*,#4227,.T.) ;
#5414 = ORIENTED_EDGE('',*,*,#4220,.T.) ;
#5415 = ORIENTED_EDGE('',*,*,#4230,.F.) ;
#5416 = ORIENTED_EDGE('',*,*,#4231,.T.) ;
#5417 = ORIENTED_EDGE('',*,*,#4232,.F.) ;
#5418 = ORIENTED_EDGE('',*,*,#4231,.F.) ;
#5419 = ORIENTED_EDGE('',*,*,#4233,.F.) ;
#5420 = ORIENTED_EDGE('',*,*,#4234,.T.) ;
#5421 = ORIENTED_EDGE('',*,*,#4235,.F.) ;
#5422 = ORIENTED_EDGE('',*,*,#4234,.F.) ;
#5423 = ORIENTED_EDGE('',*,*,#4236,.T.) ;
#5424 = ORIENTED_EDGE('',*,*,#4237,.T.) ;
#5425 = ORIENTED_EDGE('',*,*,#4238,.T.) ;
#5426 = ORIENTED_EDGE('',*,*,#4239,.T.) ;
#5427 = ORIENTED_EDGE('',*,*,#4240,.T.) ;
#5428 = ORIENTED_EDGE('',*,*,#4161,.F.) ;
#5429 = ORIENTED_EDGE('',*,*,#4241,.F.) ;
#5430 = ORIENTED_EDGE('',*,*,#4239,.F.) ;
#5431 = ORIENTED_EDGE('',*,*,#4233,.T.) ;
#5432 = ORIENTED_EDGE('',*,*,#4242,.T.) ;
#5433 = ORIENTED_EDGE('',*,*,#4162,.F.) ;
#5434 = ORIENTED_EDGE('',*,*,#4240,.F.) ;
#5435 = ORIENTED_EDGE('',*,*,#4238,.F.) ;
#5436 = ORIENTED_EDGE('',*,*,#4243,.T.) ;
#5437 = ORIENTED_EDGE('',*,*,#4163,.F.) ;
#5438 = ORIENTED_EDGE('',*,*,#4242,.F.) ;
#5439 = ORIENTED_EDGE('',*,*,#4237,.F.) ;
#5440 = ORIENTED_EDGE('',*,*,#4235,.T.) ;
#5441 = ORIENTED_EDGE('',*,*,#4241,.T.) ;
#5442 = ORIENTED_EDGE('',*,*,#4164,.F.) ;
#5443 = ORIENTED_EDGE('',*,*,#4243,.F.) ;
#5444 = ORIENTED_EDGE('',*,*,#4236,.F.) ;
#5445 = ORIENTED_EDGE('',*,*,#4244,.T.) ;
#5446 = ORIENTED_EDGE('',*,*,#4245,.T.) ;
#5447 = ORIENTED_EDGE('',*,*,#4246,.T.) ;
#5448 = ORIENTED_EDGE('',*,*,#4247,.T.) ;
#5449 = ORIENTED_EDGE('',*,*,#4248,.T.) ;
#5450 = ORIENTED_EDGE('',*,*,#4165,.F.) ;
#5451 = ORIENTED_EDGE('',*,*,#4249,.F.) ;
#5452 = ORIENTED_EDGE('',*,*,#4247,.F.) ;
#5453 = ORIENTED_EDGE('',*,*,#4230,.T.) ;
#5454 = ORIENTED_EDGE('',*,*,#4250,.T.) ;
#5455 = ORIENTED_EDGE('',*,*,#4166,.F.) ;
#5456 = ORIENTED_EDGE('',*,*,#4248,.F.) ;
#5457 = ORIENTED_EDGE('',*,*,#4246,.F.) ;
#5458 = ORIENTED_EDGE('',*,*,#4251,.T.) ;
#5459 = ORIENTED_EDGE('',*,*,#4167,.F.) ;
#5460 = ORIENTED_EDGE('',*,*,#4250,.F.) ;
#5461 = ORIENTED_EDGE('',*,*,#4245,.F.) ;
#5462 = ORIENTED_EDGE('',*,*,#4232,.T.) ;
#5463 = ORIENTED_EDGE('',*,*,#4249,.T.) ;
#5464 = ORIENTED_EDGE('',*,*,#4168,.F.) ;
#5465 = ORIENTED_EDGE('',*,*,#4251,.F.) ;
#5466 = ORIENTED_EDGE('',*,*,#4244,.F.) ;
#5467 = ORIENTED_EDGE('',*,*,#4252,.F.) ;
#5468 = ORIENTED_EDGE('',*,*,#4253,.T.) ;
#5469 = ORIENTED_EDGE('',*,*,#4169,.F.) ;
#5470 = ORIENTED_EDGE('',*,*,#4253,.F.) ;
#5471 = ORIENTED_EDGE('',*,*,#4254,.F.) ;
#5472 = ORIENTED_EDGE('',*,*,#4152,.T.) ;
#5473 = ORIENTED_EDGE('',*,*,#4158,.T.) ;
#5474 = ORIENTED_EDGE('',*,*,#4255,.F.) ;
#5475 = ORIENTED_EDGE('',*,*,#4256,.F.) ;
#5476 = ORIENTED_EDGE('',*,*,#4255,.T.) ;
#5477 = ORIENTED_EDGE('',*,*,#4157,.T.) ;
#5478 = ORIENTED_EDGE('',*,*,#4147,.F.) ;
#5479 = ORIENTED_EDGE('',*,*,#4225,.T.) ;
#5480 = ORIENTED_EDGE('',*,*,#4257,.T.) ;
#5481 = ORIENTED_EDGE('',*,*,#4212,.T.) ;
#5482 = ORIENTED_EDGE('',*,*,#4258,.T.) ;
#5483 = ORIENTED_EDGE('',*,*,#4193,.T.) ;
#5484 = ORIENTED_EDGE('',*,*,#4146,.T.) ;
#5485 = ORIENTED_EDGE('',*,*,#4153,.T.) ;
#5486 = ORIENTED_EDGE('',*,*,#4254,.T.) ;
#5487 = ORIENTED_EDGE('',*,*,#4256,.T.) ;
#5488 = ORIENTED_EDGE('',*,*,#4259,.T.) ;
#5489 = ORIENTED_EDGE('',*,*,#4191,.T.) ;
#5490 = ORIENTED_EDGE('',*,*,#4189,.T.) ;
#5491 = ORIENTED_EDGE('',*,*,#4185,.T.) ;
#5492 = ORIENTED_EDGE('',*,*,#4188,.T.) ;
#5493 = ORIENTED_EDGE('',*,*,#4195,.T.) ;
#5494 = ORIENTED_EDGE('',*,*,#4260,.T.) ;
#5495 = ORIENTED_EDGE('',*,*,#4210,.T.) ;
#5496 = ORIENTED_EDGE('',*,*,#4204,.T.) ;
#5497 = ORIENTED_EDGE('',*,*,#4207,.T.) ;
#5498 = ORIENTED_EDGE('',*,*,#4209,.T.) ;
#5499 = ORIENTED_EDGE('',*,*,#4214,.T.) ;
#5500 = ORIENTED_EDGE('',*,*,#4171,.T.) ;
#5501 = ORIENTED_EDGE('',*,*,#4174,.T.) ;
#5502 = ORIENTED_EDGE('',*,*,#4177,.T.) ;
#5503 = ORIENTED_EDGE('',*,*,#4196,.T.) ;
#5504 = ORIENTED_EDGE('',*,*,#4252,.T.) ;
#5505 = ORIENTED_EDGE('',*,*,#4211,.T.) ;
#5506 = ORIENTED_EDGE('',*,*,#4260,.F.) ;
#5507 = ORIENTED_EDGE('',*,*,#4194,.F.) ;
#5508 = ORIENTED_EDGE('',*,*,#4258,.F.) ;
#5509 = ORIENTED_EDGE('',*,*,#4192,.T.) ;
#5510 = ORIENTED_EDGE('',*,*,#4259,.F.) ;
#5511 = ORIENTED_EDGE('',*,*,#4213,.F.) ;
#5512 = ORIENTED_EDGE('',*,*,#4257,.F.) ;
#5513 = ORIENTED_EDGE('',*,*,#4261,.F.) ;
#5514 = ORIENTED_EDGE('',*,*,#4262,.T.) ;
#5515 = ORIENTED_EDGE('',*,*,#4263,.F.) ;
#5516 = ORIENTED_EDGE('',*,*,#4264,.F.) ;
#5517 = ORIENTED_EDGE('',*,*,#4265,.F.) ;
#5518 = ORIENTED_EDGE('',*,*,#4266,.F.) ;
#5519 = ORIENTED_EDGE('',*,*,#4267,.F.) ;
#5520 = ORIENTED_EDGE('',*,*,#4262,.F.) ;
#5521 = ORIENTED_EDGE('',*,*,#4268,.F.) ;
#5522 = ORIENTED_EDGE('',*,*,#4269,.F.) ;
#5523 = ORIENTED_EDGE('',*,*,#4270,.F.) ;
#5524 = ORIENTED_EDGE('',*,*,#4271,.F.) ;
#5525 = ORIENTED_EDGE('',*,*,#4266,.T.) ;
#5526 = ORIENTED_EDGE('',*,*,#4269,.T.) ;
#5527 = ORIENTED_EDGE('',*,*,#4265,.T.) ;
#5528 = ORIENTED_EDGE('',*,*,#4261,.T.) ;
#5529 = ORIENTED_EDGE('',*,*,#4272,.F.) ;
#5530 = ORIENTED_EDGE('',*,*,#4273,.F.) ;
#5531 = ORIENTED_EDGE('',*,*,#4274,.F.) ;
#5532 = ORIENTED_EDGE('',*,*,#4275,.T.) ;
#5533 = ORIENTED_EDGE('',*,*,#4276,.F.) ;
#5534 = ORIENTED_EDGE('',*,*,#4277,.T.) ;
#5535 = ORIENTED_EDGE('',*,*,#4264,.T.) ;
#5536 = ORIENTED_EDGE('',*,*,#4278,.T.) ;
#5537 = ORIENTED_EDGE('',*,*,#4272,.T.) ;
#5538 = ORIENTED_EDGE('',*,*,#4268,.T.) ;
#5539 = ORIENTED_EDGE('',*,*,#4279,.T.) ;
#5540 = ORIENTED_EDGE('',*,*,#4280,.F.) ;
#5541 = ORIENTED_EDGE('',*,*,#4279,.F.) ;
#5542 = ORIENTED_EDGE('',*,*,#4281,.F.) ;
#5543 = ORIENTED_EDGE('',*,*,#4282,.F.) ;
#5544 = ORIENTED_EDGE('',*,*,#4283,.F.) ;
#5545 = ORIENTED_EDGE('',*,*,#4284,.T.) ;
#5546 = ORIENTED_EDGE('',*,*,#4285,.F.) ;
#5547 = ORIENTED_EDGE('',*,*,#4286,.T.) ;
#5548 = ORIENTED_EDGE('',*,*,#4287,.F.) ;
#5549 = ORIENTED_EDGE('',*,*,#4288,.F.) ;
#5550 = ORIENTED_EDGE('',*,*,#4289,.F.) ;
#5551 = ORIENTED_EDGE('',*,*,#4284,.F.) ;
#5552 = ORIENTED_EDGE('',*,*,#4290,.F.) ;
#5553 = ORIENTED_EDGE('',*,*,#4286,.F.) ;
#5554 = ORIENTED_EDGE('',*,*,#4291,.F.) ;
#5555 = ORIENTED_EDGE('',*,*,#4271,.T.) ;
#5556 = ORIENTED_EDGE('',*,*,#4292,.F.) ;
#5557 = ORIENTED_EDGE('',*,*,#4287,.T.) ;
#5558 = ORIENTED_EDGE('',*,*,#4290,.T.) ;
#5559 = ORIENTED_EDGE('',*,*,#4283,.T.) ;
#5560 = ORIENTED_EDGE('',*,*,#4293,.F.) ;
#5561 = ORIENTED_EDGE('',*,*,#4294,.F.) ;
#5562 = ORIENTED_EDGE('',*,*,#4295,.F.) ;
#5563 = ORIENTED_EDGE('',*,*,#4273,.T.) ;
#5564 = ORIENTED_EDGE('',*,*,#4278,.F.) ;
#5565 = ORIENTED_EDGE('',*,*,#4263,.T.) ;
#5566 = ORIENTED_EDGE('',*,*,#4267,.T.) ;
#5567 = ORIENTED_EDGE('',*,*,#4282,.T.) ;
#5568 = ORIENTED_EDGE('',*,*,#4296,.T.) ;
#5569 = ORIENTED_EDGE('',*,*,#4293,.T.) ;
#5570 = ORIENTED_EDGE('',*,*,#4270,.T.) ;
#5571 = ORIENTED_EDGE('',*,*,#4276,.T.) ;
#5572 = ORIENTED_EDGE('',*,*,#4297,.T.) ;
#5573 = ORIENTED_EDGE('',*,*,#4298,.T.) ;
#5574 = ORIENTED_EDGE('',*,*,#4288,.T.) ;
#5575 = ORIENTED_EDGE('',*,*,#4292,.T.) ;
#5576 = ORIENTED_EDGE('',*,*,#4291,.T.) ;
#5577 = ORIENTED_EDGE('',*,*,#4299,.T.) ;
#5578 = ORIENTED_EDGE('',*,*,#4300,.F.) ;
#5579 = ORIENTED_EDGE('',*,*,#4299,.F.) ;
#5580 = ORIENTED_EDGE('',*,*,#4301,.F.) ;
#5581 = ORIENTED_EDGE('',*,*,#4302,.T.) ;
#5582 = ORIENTED_EDGE('',*,*,#4277,.F.) ;
#5583 = ORIENTED_EDGE('',*,*,#4302,.F.) ;
#5584 = ORIENTED_EDGE('',*,*,#4274,.T.) ;
#5585 = ORIENTED_EDGE('',*,*,#4295,.T.) ;
#5586 = ORIENTED_EDGE('',*,*,#4303,.T.) ;
#5587 = ORIENTED_EDGE('',*,*,#4304,.T.) ;
#5588 = ORIENTED_EDGE('',*,*,#4280,.T.) ;
#5589 = ORIENTED_EDGE('',*,*,#4300,.T.) ;
#5590 = ORIENTED_EDGE('',*,*,#4305,.T.) ;
#5591 = ORIENTED_EDGE('',*,*,#4297,.F.) ;
#5592 = ORIENTED_EDGE('',*,*,#4275,.F.) ;
#5593 = ORIENTED_EDGE('',*,*,#4304,.F.) ;
#5594 = ORIENTED_EDGE('',*,*,#4285,.T.) ;
#5595 = ORIENTED_EDGE('',*,*,#4298,.F.) ;
#5596 = ORIENTED_EDGE('',*,*,#4305,.F.) ;
#5597 = ORIENTED_EDGE('',*,*,#4303,.F.) ;
#5598 = ORIENTED_EDGE('',*,*,#4294,.T.) ;
#5599 = ORIENTED_EDGE('',*,*,#4296,.F.) ;
#5600 = ORIENTED_EDGE('',*,*,#4281,.T.) ;
#5601 = ORIENTED_EDGE('',*,*,#4289,.T.) ;
#5602 = ORIENTED_EDGE('',*,*,#4301,.T.) ;
#5603 = ORIENTED_EDGE('',*,*,#4306,.F.) ;
#5604 = ORIENTED_EDGE('',*,*,#4307,.T.) ;
#5605 = ORIENTED_EDGE('',*,*,#4308,.T.) ;
#5606 = ORIENTED_EDGE('',*,*,#4307,.F.) ;
#5607 = ORIENTED_EDGE('',*,*,#4308,.F.) ;
#5608 = ORIENTED_EDGE('',*,*,#4309,.F.) ;
#5609 = ORIENTED_EDGE('',*,*,#4310,.T.) ;
#5610 = ORIENTED_EDGE('',*,*,#4311,.T.) ;
#5611 = ORIENTED_EDGE('',*,*,#4312,.F.) ;
#5612 = ORIENTED_EDGE('',*,*,#4313,.F.) ;
#5613 = ORIENTED_EDGE('',*,*,#4312,.T.) ;
#5614 = ORIENTED_EDGE('',*,*,#4314,.T.) ;
#5615 = ORIENTED_EDGE('',*,*,#4315,.F.) ;
#5616 = ORIENTED_EDGE('',*,*,#4314,.F.) ;
#5617 = ORIENTED_EDGE('',*,*,#4311,.F.) ;
#5618 = ORIENTED_EDGE('',*,*,#4316,.F.) ;
#5619 = ORIENTED_EDGE('',*,*,#4317,.F.) ;
#5620 = ORIENTED_EDGE('',*,*,#4318,.F.) ;
#5621 = ORIENTED_EDGE('',*,*,#4315,.T.) ;
#5622 = ORIENTED_EDGE('',*,*,#4317,.T.) ;
#5623 = ORIENTED_EDGE('',*,*,#4319,.F.) ;
#5624 = ORIENTED_EDGE('',*,*,#4320,.F.) ;
#5625 = ORIENTED_EDGE('',*,*,#4319,.T.) ;
#5626 = ORIENTED_EDGE('',*,*,#4316,.T.) ;
#5627 = ORIENTED_EDGE('',*,*,#4310,.F.) ;
#5628 = ORIENTED_EDGE('',*,*,#4321,.F.) ;
#5629 = ORIENTED_EDGE('',*,*,#4322,.T.) ;
#5630 = ORIENTED_EDGE('',*,*,#4323,.T.) ;
#5631 = ORIENTED_EDGE('',*,*,#4324,.F.) ;
#5632 = ORIENTED_EDGE('',*,*,#4325,.F.) ;
#5633 = ORIENTED_EDGE('',*,*,#4324,.T.) ;
#5634 = ORIENTED_EDGE('',*,*,#4326,.T.) ;
#5635 = ORIENTED_EDGE('',*,*,#4327,.F.) ;
#5636 = ORIENTED_EDGE('',*,*,#4326,.F.) ;
#5637 = ORIENTED_EDGE('',*,*,#4323,.F.) ;
#5638 = ORIENTED_EDGE('',*,*,#4328,.F.) ;
#5639 = ORIENTED_EDGE('',*,*,#4329,.F.) ;
#5640 = ORIENTED_EDGE('',*,*,#4330,.F.) ;
#5641 = ORIENTED_EDGE('',*,*,#4327,.T.) ;
#5642 = ORIENTED_EDGE('',*,*,#4329,.T.) ;
#5643 = ORIENTED_EDGE('',*,*,#4331,.F.) ;
#5644 = ORIENTED_EDGE('',*,*,#4332,.F.) ;
#5645 = ORIENTED_EDGE('',*,*,#4331,.T.) ;
#5646 = ORIENTED_EDGE('',*,*,#4328,.T.) ;
#5647 = ORIENTED_EDGE('',*,*,#4322,.F.) ;
#5648 = ORIENTED_EDGE('',*,*,#4333,.F.) ;
#5649 = ORIENTED_EDGE('',*,*,#4334,.T.) ;
#5650 = ORIENTED_EDGE('',*,*,#4335,.T.) ;
#5651 = ORIENTED_EDGE('',*,*,#4336,.F.) ;
#5652 = ORIENTED_EDGE('',*,*,#4337,.F.) ;
#5653 = ORIENTED_EDGE('',*,*,#4336,.T.) ;
#5654 = ORIENTED_EDGE('',*,*,#4338,.T.) ;
#5655 = ORIENTED_EDGE('',*,*,#4339,.F.) ;
#5656 = ORIENTED_EDGE('',*,*,#4338,.F.) ;
#5657 = ORIENTED_EDGE('',*,*,#4335,.F.) ;
#5658 = ORIENTED_EDGE('',*,*,#4340,.F.) ;
#5659 = ORIENTED_EDGE('',*,*,#4341,.F.) ;
#5660 = ORIENTED_EDGE('',*,*,#4342,.F.) ;
#5661 = ORIENTED_EDGE('',*,*,#4339,.T.) ;
#5662 = ORIENTED_EDGE('',*,*,#4341,.T.) ;
#5663 = ORIENTED_EDGE('',*,*,#4343,.F.) ;
#5664 = ORIENTED_EDGE('',*,*,#4344,.F.) ;
#5665 = ORIENTED_EDGE('',*,*,#4343,.T.) ;
#5666 = ORIENTED_EDGE('',*,*,#4340,.T.) ;
#5667 = ORIENTED_EDGE('',*,*,#4334,.F.) ;
#5668 = ORIENTED_EDGE('',*,*,#4345,.T.) ;
#5669 = ORIENTED_EDGE('',*,*,#4346,.T.) ;
#5670 = ORIENTED_EDGE('',*,*,#4347,.F.) ;
#5671 = ORIENTED_EDGE('',*,*,#4346,.F.) ;
#5672 = ORIENTED_EDGE('',*,*,#4348,.F.) ;
#5673 = ORIENTED_EDGE('',*,*,#4349,.T.) ;
#5674 = ORIENTED_EDGE('',*,*,#4350,.T.) ;
#5675 = ORIENTED_EDGE('',*,*,#4349,.F.) ;
#5676 = ORIENTED_EDGE('',*,*,#4350,.F.) ;
#5677 = ORIENTED_EDGE('',*,*,#4345,.F.) ;
#5678 = ORIENTED_EDGE('',*,*,#4351,.T.) ;
#5679 = ORIENTED_EDGE('',*,*,#4348,.T.) ;
#5680 = ORIENTED_EDGE('',*,*,#4352,.T.) ;
#5681 = ORIENTED_EDGE('',*,*,#4353,.T.) ;
#5682 = ORIENTED_EDGE('',*,*,#4351,.F.) ;
#5683 = ORIENTED_EDGE('',*,*,#4353,.F.) ;
#5684 = ORIENTED_EDGE('',*,*,#4354,.F.) ;
#5685 = ORIENTED_EDGE('',*,*,#4355,.T.) ;
#5686 = ORIENTED_EDGE('',*,*,#4356,.T.) ;
#5687 = ORIENTED_EDGE('',*,*,#4355,.F.) ;
#5688 = ORIENTED_EDGE('',*,*,#4356,.F.) ;
#5689 = ORIENTED_EDGE('',*,*,#4352,.F.) ;
#5690 = ORIENTED_EDGE('',*,*,#4357,.T.) ;
#5691 = ORIENTED_EDGE('',*,*,#4354,.T.) ;
#5692 = ORIENTED_EDGE('',*,*,#4358,.F.) ;
#5693 = ORIENTED_EDGE('',*,*,#4359,.T.) ;
#5694 = ORIENTED_EDGE('',*,*,#4357,.F.) ;
#5695 = ORIENTED_EDGE('',*,*,#4359,.F.) ;
#5696 = ORIENTED_EDGE('',*,*,#4347,.T.) ;
#5697 = ORIENTED_EDGE('',*,*,#4306,.T.) ;
#5698 = ORIENTED_EDGE('',*,*,#4358,.T.) ;
#5699 = ORIENTED_EDGE('',*,*,#4318,.T.) ;
#5700 = ORIENTED_EDGE('',*,*,#4320,.T.) ;
#5701 = ORIENTED_EDGE('',*,*,#4309,.T.) ;
#5702 = ORIENTED_EDGE('',*,*,#4313,.T.) ;
#5703 = ORIENTED_EDGE('',*,*,#4330,.T.) ;
#5704 = ORIENTED_EDGE('',*,*,#4332,.T.) ;
#5705 = ORIENTED_EDGE('',*,*,#4321,.T.) ;
#5706 = ORIENTED_EDGE('',*,*,#4325,.T.) ;
#5707 = ORIENTED_EDGE('',*,*,#4342,.T.) ;
#5708 = ORIENTED_EDGE('',*,*,#4344,.T.) ;
#5709 = ORIENTED_EDGE('',*,*,#4333,.T.) ;
#5710 = ORIENTED_EDGE('',*,*,#4337,.T.) ;
#5711 = ORIENTED_EDGE('',*,*,#4360,.F.) ;
#5712 = ORIENTED_EDGE('',*,*,#4361,.T.) ;
#5713 = ORIENTED_EDGE('',*,*,#4362,.F.) ;
#5714 = ORIENTED_EDGE('',*,*,#4361,.F.) ;
#5715 = ORIENTED_EDGE('',*,*,#4363,.F.) ;
#5716 = ORIENTED_EDGE('',*,*,#4364,.T.) ;
#5717 = ORIENTED_EDGE('',*,*,#4365,.F.) ;
#5718 = ORIENTED_EDGE('',*,*,#4364,.F.) ;
#5719 = ORIENTED_EDGE('',*,*,#4365,.T.) ;
#5720 = ORIENTED_EDGE('',*,*,#4360,.T.) ;
#5721 = ORIENTED_EDGE('',*,*,#4363,.T.) ;
#5722 = ORIENTED_EDGE('',*,*,#4362,.T.) ;
#5723 = ORIENTED_EDGE('',*,*,#4366,.F.) ;
#5724 = ORIENTED_EDGE('',*,*,#4367,.T.) ;
#5725 = ORIENTED_EDGE('',*,*,#4368,.F.) ;
#5726 = ORIENTED_EDGE('',*,*,#4367,.F.) ;
#5727 = ORIENTED_EDGE('',*,*,#4369,.F.) ;
#5728 = ORIENTED_EDGE('',*,*,#4370,.T.) ;
#5729 = ORIENTED_EDGE('',*,*,#4371,.F.) ;
#5730 = ORIENTED_EDGE('',*,*,#4370,.F.) ;
#5731 = ORIENTED_EDGE('',*,*,#4371,.T.) ;
#5732 = ORIENTED_EDGE('',*,*,#4366,.T.) ;
#5733 = ORIENTED_EDGE('',*,*,#4369,.T.) ;
#5734 = ORIENTED_EDGE('',*,*,#4368,.T.) ;
#5735 = ORIENTED_EDGE('',*,*,#4372,.T.) ;
#5736 = ORIENTED_EDGE('',*,*,#4373,.T.) ;
#5737 = ORIENTED_EDGE('',*,*,#4373,.F.) ;
#5738 = ORIENTED_EDGE('',*,*,#4374,.F.) ;
#5739 = ORIENTED_EDGE('',*,*,#4375,.T.) ;
#5740 = ORIENTED_EDGE('',*,*,#4372,.F.) ;
#5741 = ORIENTED_EDGE('',*,*,#4375,.F.) ;
#5742 = ORIENTED_EDGE('',*,*,#4374,.T.) ;
#5743 = ORIENTED_EDGE('',*,*,#4376,.F.) ;
#5744 = ORIENTED_EDGE('',*,*,#4377,.T.) ;
#5745 = ORIENTED_EDGE('',*,*,#4378,.F.) ;
#5746 = ORIENTED_EDGE('',*,*,#4377,.F.) ;
#5747 = ORIENTED_EDGE('',*,*,#4379,.F.) ;
#5748 = ORIENTED_EDGE('',*,*,#4380,.T.) ;
#5749 = ORIENTED_EDGE('',*,*,#4381,.F.) ;
#5750 = ORIENTED_EDGE('',*,*,#4380,.F.) ;
#5751 = ORIENTED_EDGE('',*,*,#4382,.T.) ;
#5752 = ORIENTED_EDGE('',*,*,#4381,.T.) ;
#5753 = ORIENTED_EDGE('',*,*,#4382,.F.) ;
#5754 = ORIENTED_EDGE('',*,*,#4383,.T.) ;
#5755 = ORIENTED_EDGE('',*,*,#4384,.F.) ;
#5756 = ORIENTED_EDGE('',*,*,#4383,.F.) ;
#5757 = ORIENTED_EDGE('',*,*,#4384,.T.) ;
#5758 = ORIENTED_EDGE('',*,*,#4376,.T.) ;
#5759 = ORIENTED_EDGE('',*,*,#4379,.T.) ;
#5760 = ORIENTED_EDGE('',*,*,#4378,.T.) ;
#5761 = ORIENTED_EDGE('',*,*,#4385,.F.) ;
#5762 = ORIENTED_EDGE('',*,*,#4386,.T.) ;
#5763 = ORIENTED_EDGE('',*,*,#4387,.F.) ;
#5764 = ORIENTED_EDGE('',*,*,#4386,.F.) ;
#5765 = ORIENTED_EDGE('',*,*,#4385,.T.) ;
#5766 = ORIENTED_EDGE('',*,*,#4388,.F.) ;
#5767 = ORIENTED_EDGE('',*,*,#4389,.T.) ;
#5768 = ORIENTED_EDGE('',*,*,#4390,.F.) ;
#5769 = ORIENTED_EDGE('',*,*,#4389,.F.) ;
#5770 = ORIENTED_EDGE('',*,*,#4390,.T.) ;
#5771 = ORIENTED_EDGE('',*,*,#4388,.T.) ;
#5772 = ORIENTED_EDGE('',*,*,#4387,.T.) ;
#5773 = ORIENTED_EDGE('',*,*,#4391,.F.) ;
#5774 = ORIENTED_EDGE('',*,*,#4392,.T.) ;
#5775 = ORIENTED_EDGE('',*,*,#4393,.F.) ;
#5776 = ORIENTED_EDGE('',*,*,#4392,.F.) ;
#5777 = ORIENTED_EDGE('',*,*,#4393,.T.) ;
#5778 = ORIENTED_EDGE('',*,*,#4391,.T.) ;
#5779 = ORIENTED_EDGE('',*,*,#4394,.F.) ;
#5780 = ORIENTED_EDGE('',*,*,#4395,.F.) ;
#5781 = ORIENTED_EDGE('',*,*,#4396,.F.) ;
#5782 = ORIENTED_EDGE('',*,*,#4397,.F.) ;
#5783 = ORIENTED_EDGE('',*,*,#4398,.F.) ;
#5784 = ORIENTED_EDGE('',*,*,#4399,.T.) ;
#5785 = ORIENTED_EDGE('',*,*,#4400,.T.) ;
#5786 = ORIENTED_EDGE('',*,*,#4401,.F.) ;
#5787 = ORIENTED_EDGE('',*,*,#4402,.F.) ;
#5788 = ORIENTED_EDGE('',*,*,#4403,.F.) ;
#5789 = ORIENTED_EDGE('',*,*,#4399,.F.) ;
#5790 = ORIENTED_EDGE('',*,*,#4404,.F.) ;
#5791 = ORIENTED_EDGE('',*,*,#4405,.T.) ;
#5792 = ORIENTED_EDGE('',*,*,#4402,.T.) ;
#5793 = ORIENTED_EDGE('',*,*,#4406,.F.) ;
#5794 = ORIENTED_EDGE('',*,*,#4407,.T.) ;
#5795 = ORIENTED_EDGE('',*,*,#4395,.T.) ;
#5796 = ORIENTED_EDGE('',*,*,#4408,.F.) ;
#5797 = ORIENTED_EDGE('',*,*,#4397,.T.) ;
#5798 = ORIENTED_EDGE('',*,*,#4409,.T.) ;
#5799 = ORIENTED_EDGE('',*,*,#4410,.F.) ;
#5800 = ORIENTED_EDGE('',*,*,#4409,.F.) ;
#5801 = ORIENTED_EDGE('',*,*,#4396,.T.) ;
#5802 = ORIENTED_EDGE('',*,*,#4407,.F.) ;
#5803 = ORIENTED_EDGE('',*,*,#4411,.F.) ;
#5804 = ORIENTED_EDGE('',*,*,#4400,.F.) ;
#5805 = ORIENTED_EDGE('',*,*,#4403,.T.) ;
#5806 = ORIENTED_EDGE('',*,*,#4405,.F.) ;
#5807 = ORIENTED_EDGE('',*,*,#4412,.F.) ;
#5808 = ORIENTED_EDGE('',*,*,#4413,.T.) ;
#5809 = ORIENTED_EDGE('',*,*,#4414,.F.) ;
#5810 = ORIENTED_EDGE('',*,*,#4413,.F.) ;
#5811 = ORIENTED_EDGE('',*,*,#4415,.F.) ;
#5812 = ORIENTED_EDGE('',*,*,#4416,.F.) ;
#5813 = ORIENTED_EDGE('',*,*,#4417,.F.) ;
#5814 = ORIENTED_EDGE('',*,*,#4418,.F.) ;
#5815 = ORIENTED_EDGE('',*,*,#4419,.T.) ;
#5816 = ORIENTED_EDGE('',*,*,#4420,.F.) ;
#5817 = ORIENTED_EDGE('',*,*,#4419,.F.) ;
#5818 = ORIENTED_EDGE('',*,*,#4421,.F.) ;
#5819 = ORIENTED_EDGE('',*,*,#4422,.F.) ;
#5820 = ORIENTED_EDGE('',*,*,#4416,.T.) ;
#5821 = ORIENTED_EDGE('',*,*,#4423,.F.) ;
#5822 = ORIENTED_EDGE('',*,*,#4424,.T.) ;
#5823 = ORIENTED_EDGE('',*,*,#4425,.F.) ;
#5824 = ORIENTED_EDGE('',*,*,#4417,.T.) ;
#5825 = ORIENTED_EDGE('',*,*,#4415,.T.) ;
#5826 = ORIENTED_EDGE('',*,*,#4422,.T.) ;
#5827 = ORIENTED_EDGE('',*,*,#4426,.F.) ;
#5828 = ORIENTED_EDGE('',*,*,#4424,.F.) ;
#5829 = ORIENTED_EDGE('',*,*,#4406,.T.) ;
#5830 = ORIENTED_EDGE('',*,*,#4394,.T.) ;
#5831 = ORIENTED_EDGE('',*,*,#4408,.T.) ;
#5832 = ORIENTED_EDGE('',*,*,#4410,.T.) ;
#5833 = ORIENTED_EDGE('',*,*,#4421,.T.) ;
#5834 = ORIENTED_EDGE('',*,*,#4418,.T.) ;
#5835 = ORIENTED_EDGE('',*,*,#4425,.T.) ;
#5836 = ORIENTED_EDGE('',*,*,#4426,.T.) ;
#5837 = ORIENTED_EDGE('',*,*,#4412,.T.) ;
#5838 = ORIENTED_EDGE('',*,*,#4427,.T.) ;
#5839 = ORIENTED_EDGE('',*,*,#4414,.T.) ;
#5840 = ORIENTED_EDGE('',*,*,#4420,.T.) ;
#5841 = ORIENTED_EDGE('',*,*,#4427,.F.) ;
#5842 = ORIENTED_EDGE('',*,*,#4428,.T.) ;
#5843 = ORIENTED_EDGE('',*,*,#4429,.F.) ;
#5844 = ORIENTED_EDGE('',*,*,#4428,.F.) ;
#5845 = ORIENTED_EDGE('',*,*,#4404,.T.) ;
#5846 = ORIENTED_EDGE('',*,*,#4401,.T.) ;
#5847 = ORIENTED_EDGE('',*,*,#4398,.T.) ;
#5848 = ORIENTED_EDGE('',*,*,#4411,.T.) ;
#5849 = ORIENTED_EDGE('',*,*,#4429,.T.) ;
#5850 = ORIENTED_EDGE('',*,*,#4423,.T.) ;
#5851 = ORIENTED_EDGE('',*,*,#4430,.T.) ;
#5852 = ORIENTED_EDGE('',*,*,#4430,.F.) ;
#5853 = ORIENTED_EDGE('',*,*,#4431,.F.) ;
#5854 = ORIENTED_EDGE('',*,*,#4432,.F.) ;
#5855 = ORIENTED_EDGE('',*,*,#4432,.T.) ;
#5856 = ORIENTED_EDGE('',*,*,#4433,.T.) ;
#5857 = ORIENTED_EDGE('',*,*,#4431,.T.) ;
#5858 = ORIENTED_EDGE('',*,*,#4433,.F.) ;
#5859 = ORIENTED_EDGE('',*,*,#4434,.T.) ;
#5860 = ORIENTED_EDGE('',*,*,#4435,.T.) ;
#5861 = ORIENTED_EDGE('',*,*,#4436,.T.) ;
#5862 = ORIENTED_EDGE('',*,*,#4437,.F.) ;
#5863 = ORIENTED_EDGE('',*,*,#4438,.T.) ;
#5864 = ORIENTED_EDGE('',*,*,#4439,.F.) ;
#5865 = ORIENTED_EDGE('',*,*,#4440,.T.) ;
#5866 = ORIENTED_EDGE('',*,*,#4434,.F.) ;
#5867 = ORIENTED_EDGE('',*,*,#4440,.F.) ;
#5868 = ORIENTED_EDGE('',*,*,#4441,.F.) ;
#5869 = ORIENTED_EDGE('',*,*,#4442,.T.) ;
#5870 = ORIENTED_EDGE('',*,*,#4443,.T.) ;
#5871 = ORIENTED_EDGE('',*,*,#4444,.F.) ;
#5872 = ORIENTED_EDGE('',*,*,#4445,.F.) ;
#5873 = ORIENTED_EDGE('',*,*,#4442,.F.) ;
#5874 = ORIENTED_EDGE('',*,*,#4446,.T.) ;
#5875 = ORIENTED_EDGE('',*,*,#4447,.F.) ;
#5876 = ORIENTED_EDGE('',*,*,#4438,.F.) ;
#5877 = ORIENTED_EDGE('',*,*,#4448,.F.) ;
#5878 = ORIENTED_EDGE('',*,*,#4446,.F.) ;
#5879 = ORIENTED_EDGE('',*,*,#4449,.T.) ;
#5880 = ORIENTED_EDGE('',*,*,#4450,.T.) ;
#5881 = ORIENTED_EDGE('',*,*,#4443,.F.) ;
#5882 = ORIENTED_EDGE('',*,*,#4450,.F.) ;
#5883 = ORIENTED_EDGE('',*,*,#4451,.T.) ;
#5884 = ORIENTED_EDGE('',*,*,#4436,.F.) ;
#5885 = ORIENTED_EDGE('',*,*,#4435,.F.) ;
#5886 = ORIENTED_EDGE('',*,*,#4452,.T.) ;
#5887 = ORIENTED_EDGE('',*,*,#4453,.T.) ;
#5888 = ORIENTED_EDGE('',*,*,#4444,.T.) ;
#5889 = ORIENTED_EDGE('',*,*,#4454,.T.) ;
#5890 = ORIENTED_EDGE('',*,*,#4452,.F.) ;
#5891 = ORIENTED_EDGE('',*,*,#4447,.T.) ;
#5892 = ORIENTED_EDGE('',*,*,#4448,.T.) ;
#5893 = ORIENTED_EDGE('',*,*,#4441,.T.) ;
#5894 = ORIENTED_EDGE('',*,*,#4439,.T.) ;
#5895 = ORIENTED_EDGE('',*,*,#4449,.F.) ;
#5896 = ORIENTED_EDGE('',*,*,#4437,.T.) ;
#5897 = ORIENTED_EDGE('',*,*,#4451,.F.) ;
#5898 = ORIENTED_EDGE('',*,*,#4445,.T.) ;
#5899 = ORIENTED_EDGE('',*,*,#4453,.F.) ;
#5900 = ORIENTED_EDGE('',*,*,#4454,.F.) ;
#5901 = ORIENTED_EDGE('',*,*,#4455,.F.) ;
#5902 = ORIENTED_EDGE('',*,*,#4456,.T.) ;
#5903 = ORIENTED_EDGE('',*,*,#4457,.F.) ;
#5904 = ORIENTED_EDGE('',*,*,#4456,.F.) ;
#5905 = ORIENTED_EDGE('',*,*,#4458,.F.) ;
#5906 = ORIENTED_EDGE('',*,*,#4459,.T.) ;
#5907 = ORIENTED_EDGE('',*,*,#4460,.F.) ;
#5908 = ORIENTED_EDGE('',*,*,#4459,.F.) ;
#5909 = ORIENTED_EDGE('',*,*,#4460,.T.) ;
#5910 = ORIENTED_EDGE('',*,*,#4455,.T.) ;
#5911 = ORIENTED_EDGE('',*,*,#4458,.T.) ;
#5912 = ORIENTED_EDGE('',*,*,#4457,.T.) ;
#5913 = ORIENTED_EDGE('',*,*,#4461,.F.) ;
#5914 = ORIENTED_EDGE('',*,*,#4462,.T.) ;
#5915 = ORIENTED_EDGE('',*,*,#4463,.F.) ;
#5916 = ORIENTED_EDGE('',*,*,#4462,.F.) ;
#5917 = ORIENTED_EDGE('',*,*,#4464,.F.) ;
#5918 = ORIENTED_EDGE('',*,*,#4465,.T.) ;
#5919 = ORIENTED_EDGE('',*,*,#4466,.F.) ;
#5920 = ORIENTED_EDGE('',*,*,#4465,.F.) ;
#5921 = ORIENTED_EDGE('',*,*,#4467,.T.) ;
#5922 = ORIENTED_EDGE('',*,*,#4466,.T.) ;
#5923 = ORIENTED_EDGE('',*,*,#4467,.F.) ;
#5924 = ORIENTED_EDGE('',*,*,#4468,.T.) ;
#5925 = ORIENTED_EDGE('',*,*,#4469,.F.) ;
#5926 = ORIENTED_EDGE('',*,*,#4468,.F.) ;
#5927 = ORIENTED_EDGE('',*,*,#4469,.T.) ;
#5928 = ORIENTED_EDGE('',*,*,#4461,.T.) ;
#5929 = ORIENTED_EDGE('',*,*,#4464,.T.) ;
#5930 = ORIENTED_EDGE('',*,*,#4463,.T.) ;
#5931 = ORIENTED_EDGE('',*,*,#4470,.F.) ;
#5932 = ORIENTED_EDGE('',*,*,#4471,.T.) ;
#5933 = ORIENTED_EDGE('',*,*,#4472,.F.) ;
#5934 = ORIENTED_EDGE('',*,*,#4471,.F.) ;
#5935 = ORIENTED_EDGE('',*,*,#4472,.T.) ;
#5936 = ORIENTED_EDGE('',*,*,#4470,.T.) ;
#5937 = ORIENTED_EDGE('',*,*,#4473,.F.) ;
#5938 = ORIENTED_EDGE('',*,*,#4474,.T.) ;
#5939 = ORIENTED_EDGE('',*,*,#4475,.F.) ;
#5940 = ORIENTED_EDGE('',*,*,#4474,.F.) ;
#5941 = ORIENTED_EDGE('',*,*,#4475,.T.) ;
#5942 = ORIENTED_EDGE('',*,*,#4473,.T.) ;
#5943 = ORIENTED_EDGE('',*,*,#4476,.F.) ;
#5944 = ORIENTED_EDGE('',*,*,#4477,.T.) ;
#5945 = ORIENTED_EDGE('',*,*,#4478,.F.) ;
#5946 = ORIENTED_EDGE('',*,*,#4477,.F.) ;
#5947 = ORIENTED_EDGE('',*,*,#4479,.T.) ;
#5948 = ORIENTED_EDGE('',*,*,#4480,.T.) ;
#5949 = ORIENTED_EDGE('',*,*,#4481,.T.) ;
#5950 = ORIENTED_EDGE('',*,*,#4482,.T.) ;
#5951 = ORIENTED_EDGE('',*,*,#4483,.T.) ;
#5952 = ORIENTED_EDGE('',*,*,#4481,.F.) ;
#5953 = ORIENTED_EDGE('',*,*,#4484,.F.) ;
#5954 = ORIENTED_EDGE('',*,*,#4485,.F.) ;
#5955 = ORIENTED_EDGE('',*,*,#4486,.F.) ;
#5956 = ORIENTED_EDGE('',*,*,#4487,.T.) ;
#5957 = ORIENTED_EDGE('',*,*,#4479,.F.) ;
#5958 = ORIENTED_EDGE('',*,*,#4488,.F.) ;
#5959 = ORIENTED_EDGE('',*,*,#4489,.F.) ;
#5960 = ORIENTED_EDGE('',*,*,#4490,.T.) ;
#5961 = ORIENTED_EDGE('',*,*,#4491,.F.) ;
#5962 = ORIENTED_EDGE('',*,*,#4492,.F.) ;
#5963 = ORIENTED_EDGE('',*,*,#4493,.F.) ;
#5964 = ORIENTED_EDGE('',*,*,#4494,.T.) ;
#5965 = ORIENTED_EDGE('',*,*,#4495,.F.) ;
#5966 = ORIENTED_EDGE('',*,*,#4484,.T.) ;
#5967 = ORIENTED_EDGE('',*,*,#4480,.F.) ;
#5968 = ORIENTED_EDGE('',*,*,#4487,.F.) ;
#5969 = ORIENTED_EDGE('',*,*,#4496,.T.) ;
#5970 = ORIENTED_EDGE('',*,*,#4486,.T.) ;
#5971 = ORIENTED_EDGE('',*,*,#4497,.T.) ;
#5972 = ORIENTED_EDGE('',*,*,#4498,.T.) ;
#5973 = ORIENTED_EDGE('',*,*,#4489,.T.) ;
#5974 = ORIENTED_EDGE('',*,*,#4496,.F.) ;
#5975 = ORIENTED_EDGE('',*,*,#4499,.T.) ;
#5976 = ORIENTED_EDGE('',*,*,#4500,.F.) ;
#5977 = ORIENTED_EDGE('',*,*,#4499,.F.) ;
#5978 = ORIENTED_EDGE('',*,*,#4498,.F.) ;
#5979 = ORIENTED_EDGE('',*,*,#4501,.F.) ;
#5980 = ORIENTED_EDGE('',*,*,#4502,.F.) ;
#5981 = ORIENTED_EDGE('',*,*,#4490,.F.) ;
#5982 = ORIENTED_EDGE('',*,*,#4503,.F.) ;
#5983 = ORIENTED_EDGE('',*,*,#4494,.F.) ;
#5984 = ORIENTED_EDGE('',*,*,#4504,.F.) ;
#5985 = ORIENTED_EDGE('',*,*,#4505,.F.) ;
#5986 = ORIENTED_EDGE('',*,*,#4504,.T.) ;
#5987 = ORIENTED_EDGE('',*,*,#4493,.T.) ;
#5988 = ORIENTED_EDGE('',*,*,#4506,.T.) ;
#5989 = ORIENTED_EDGE('',*,*,#4507,.T.) ;
#5990 = ORIENTED_EDGE('',*,*,#4478,.T.) ;
#5991 = ORIENTED_EDGE('',*,*,#4495,.T.) ;
#5992 = ORIENTED_EDGE('',*,*,#4503,.T.) ;
#5993 = ORIENTED_EDGE('',*,*,#4508,.T.) ;
#5994 = ORIENTED_EDGE('',*,*,#4485,.T.) ;
#5995 = ORIENTED_EDGE('',*,*,#4508,.F.) ;
#5996 = ORIENTED_EDGE('',*,*,#4505,.T.) ;
#5997 = ORIENTED_EDGE('',*,*,#4507,.F.) ;
#5998 = ORIENTED_EDGE('',*,*,#4509,.T.) ;
#5999 = ORIENTED_EDGE('',*,*,#4510,.F.) ;
#6000 = ORIENTED_EDGE('',*,*,#4501,.T.) ;
#6001 = ORIENTED_EDGE('',*,*,#4497,.F.) ;
#6002 = ORIENTED_EDGE('',*,*,#4488,.T.) ;
#6003 = ORIENTED_EDGE('',*,*,#4482,.F.) ;
#6004 = ORIENTED_EDGE('',*,*,#4483,.F.) ;
#6005 = ORIENTED_EDGE('',*,*,#4500,.T.) ;
#6006 = ORIENTED_EDGE('',*,*,#4502,.T.) ;
#6007 = ORIENTED_EDGE('',*,*,#4510,.T.) ;
#6008 = ORIENTED_EDGE('',*,*,#4511,.T.) ;
#6009 = ORIENTED_EDGE('',*,*,#4491,.T.) ;
#6010 = ORIENTED_EDGE('',*,*,#4476,.T.) ;
#6011 = ORIENTED_EDGE('',*,*,#4492,.T.) ;
#6012 = ORIENTED_EDGE('',*,*,#4511,.F.) ;
#6013 = ORIENTED_EDGE('',*,*,#4509,.F.) ;
#6014 = ORIENTED_EDGE('',*,*,#4506,.F.) ;
#6015 = ORIENTED_EDGE('',*,*,#4512,.T.) ;
#6016 = ORIENTED_EDGE('',*,*,#4513,.T.) ;
#6017 = ORIENTED_EDGE('',*,*,#4512,.F.) ;
#6018 = ORIENTED_EDGE('',*,*,#4514,.T.) ;
#6019 = ORIENTED_EDGE('',*,*,#4515,.F.) ;
#6020 = ORIENTED_EDGE('',*,*,#4514,.F.) ;
#6021 = ORIENTED_EDGE('',*,*,#4515,.T.) ;
#6022 = ORIENTED_EDGE('',*,*,#4516,.F.) ;
#6023 = ORIENTED_EDGE('',*,*,#4517,.T.) ;
#6024 = ORIENTED_EDGE('',*,*,#4513,.F.) ;
#6025 = ORIENTED_EDGE('',*,*,#4517,.F.) ;
#6026 = ORIENTED_EDGE('',*,*,#4516,.T.) ;
#6027 = ORIENTED_EDGE('',*,*,#4518,.T.) ;
#6028 = ORIENTED_EDGE('',*,*,#4519,.T.) ;
#6029 = ORIENTED_EDGE('',*,*,#4520,.T.) ;
#6030 = ORIENTED_EDGE('',*,*,#4521,.T.) ;
#6031 = ORIENTED_EDGE('',*,*,#4522,.T.) ;
#6032 = ORIENTED_EDGE('',*,*,#4523,.T.) ;
#6033 = ORIENTED_EDGE('',*,*,#4524,.T.) ;
#6034 = ORIENTED_EDGE('',*,*,#4525,.T.) ;
#6035 = ORIENTED_EDGE('',*,*,#4526,.T.) ;
#6036 = ORIENTED_EDGE('',*,*,#4527,.T.) ;
#6037 = ORIENTED_EDGE('',*,*,#4528,.T.) ;
#6038 = ORIENTED_EDGE('',*,*,#4529,.T.) ;
#6039 = ORIENTED_EDGE('',*,*,#4530,.T.) ;
#6040 = ORIENTED_EDGE('',*,*,#4531,.T.) ;
#6041 = ORIENTED_EDGE('',*,*,#4532,.T.) ;
#6042 = ORIENTED_EDGE('',*,*,#4533,.T.) ;
#6043 = ORIENTED_EDGE('',*,*,#4534,.T.) ;
#6044 = ORIENTED_EDGE('',*,*,#4535,.T.) ;
#6045 = ORIENTED_EDGE('',*,*,#4536,.T.) ;
#6046 = ORIENTED_EDGE('',*,*,#4537,.T.) ;
#6047 = ORIENTED_EDGE('',*,*,#4538,.T.) ;
#6048 = ORIENTED_EDGE('',*,*,#4539,.T.) ;
#6049 = ORIENTED_EDGE('',*,*,#4540,.T.) ;
#6050 = ORIENTED_EDGE('',*,*,#4541,.T.) ;
#6051 = ORIENTED_EDGE('',*,*,#4542,.T.) ;
#6052 = ORIENTED_EDGE('',*,*,#4543,.T.) ;
#6053 = ORIENTED_EDGE('',*,*,#4544,.T.) ;
#6054 = ORIENTED_EDGE('',*,*,#4545,.T.) ;
#6055 = ORIENTED_EDGE('',*,*,#4546,.T.) ;
#6056 = ORIENTED_EDGE('',*,*,#4547,.T.) ;
#6057 = ORIENTED_EDGE('',*,*,#4548,.T.) ;
#6058 = ORIENTED_EDGE('',*,*,#4549,.T.) ;
#6059 = ORIENTED_EDGE('',*,*,#4550,.T.) ;
#6060 = ORIENTED_EDGE('',*,*,#4551,.T.) ;
#6061 = ORIENTED_EDGE('',*,*,#4552,.T.) ;
#6062 = ORIENTED_EDGE('',*,*,#4553,.T.) ;
#6063 = ORIENTED_EDGE('',*,*,#4554,.T.) ;
#6064 = ORIENTED_EDGE('',*,*,#4555,.T.) ;
#6065 = ORIENTED_EDGE('',*,*,#4556,.T.) ;
#6066 = ORIENTED_EDGE('',*,*,#4557,.T.) ;
#6067 = ORIENTED_EDGE('',*,*,#4558,.T.) ;
#6068 = ORIENTED_EDGE('',*,*,#4559,.T.) ;
#6069 = ORIENTED_EDGE('',*,*,#4560,.T.) ;
#6070 = ORIENTED_EDGE('',*,*,#4561,.T.) ;
#6071 = ORIENTED_EDGE('',*,*,#4562,.T.) ;
#6072 = ORIENTED_EDGE('',*,*,#4563,.T.) ;
#6073 = ORIENTED_EDGE('',*,*,#4564,.T.) ;
#6074 = ORIENTED_EDGE('',*,*,#4565,.T.) ;
#6075 = ORIENTED_EDGE('',*,*,#4566,.T.) ;
#6076 = ORIENTED_EDGE('',*,*,#4567,.T.) ;
#6077 = ORIENTED_EDGE('',*,*,#4568,.T.) ;
#6078 = ORIENTED_EDGE('',*,*,#4569,.T.) ;
#6079 = ORIENTED_EDGE('',*,*,#4570,.T.) ;
#6080 = ORIENTED_EDGE('',*,*,#4571,.T.) ;
#6081 = ORIENTED_EDGE('',*,*,#4572,.T.) ;
#6082 = ORIENTED_EDGE('',*,*,#4573,.T.) ;
#6083 = ORIENTED_EDGE('',*,*,#4574,.T.) ;
#6084 = ORIENTED_EDGE('',*,*,#4575,.T.) ;
#6085 = ORIENTED_EDGE('',*,*,#4576,.T.) ;
#6086 = ORIENTED_EDGE('',*,*,#4577,.T.) ;
#6087 = ORIENTED_EDGE('',*,*,#4578,.T.) ;
#6088 = ORIENTED_EDGE('',*,*,#4579,.T.) ;
#6089 = ORIENTED_EDGE('',*,*,#4580,.T.) ;
#6090 = ORIENTED_EDGE('',*,*,#4581,.T.) ;
#6091 = ORIENTED_EDGE('',*,*,#4582,.T.) ;
#6092 = ORIENTED_EDGE('',*,*,#4583,.T.) ;
#6093 = ORIENTED_EDGE('',*,*,#4584,.T.) ;
#6094 = ORIENTED_EDGE('',*,*,#4585,.T.) ;
#6095 = ORIENTED_EDGE('',*,*,#4586,.T.) ;
#6096 = ORIENTED_EDGE('',*,*,#4587,.T.) ;
#6097 = ORIENTED_EDGE('',*,*,#4588,.T.) ;
#6098 = ORIENTED_EDGE('',*,*,#4589,.T.) ;
#6099 = ORIENTED_EDGE('',*,*,#4590,.T.) ;
#6100 = ORIENTED_EDGE('',*,*,#4591,.T.) ;
#6101 = ORIENTED_EDGE('',*,*,#4592,.T.) ;
#6102 = ORIENTED_EDGE('',*,*,#4593,.T.) ;
#6103 = ORIENTED_EDGE('',*,*,#4594,.T.) ;
#6104 = ORIENTED_EDGE('',*,*,#4595,.T.) ;
#6105 = ORIENTED_EDGE('',*,*,#4596,.T.) ;
#6106 = ORIENTED_EDGE('',*,*,#4597,.T.) ;
#6107 = ORIENTED_EDGE('',*,*,#4598,.T.) ;
#6108 = ORIENTED_EDGE('',*,*,#4599,.T.) ;
#6109 = ORIENTED_EDGE('',*,*,#4600,.T.) ;
#6110 = ORIENTED_EDGE('',*,*,#4601,.T.) ;
#6111 = ORIENTED_EDGE('',*,*,#4602,.T.) ;
#6112 = ORIENTED_EDGE('',*,*,#4603,.T.) ;
#6113 = ORIENTED_EDGE('',*,*,#4604,.T.) ;
#6114 = ORIENTED_EDGE('',*,*,#4605,.T.) ;
#6115 = ORIENTED_EDGE('',*,*,#4606,.T.) ;
#6116 = ORIENTED_EDGE('',*,*,#4607,.T.) ;
#6117 = ORIENTED_EDGE('',*,*,#4608,.T.) ;
#6118 = ORIENTED_EDGE('',*,*,#4609,.T.) ;
#6119 = ORIENTED_EDGE('',*,*,#4610,.T.) ;
#6120 = ORIENTED_EDGE('',*,*,#4611,.T.) ;
#6121 = ORIENTED_EDGE('',*,*,#4612,.T.) ;
#6122 = ORIENTED_EDGE('',*,*,#4613,.T.) ;
#6123 = ORIENTED_EDGE('',*,*,#4614,.T.) ;
#6124 = ORIENTED_EDGE('',*,*,#4615,.T.) ;
#6125 = ORIENTED_EDGE('',*,*,#4616,.T.) ;
#6126 = ORIENTED_EDGE('',*,*,#4617,.T.) ;
#6127 = ORIENTED_EDGE('',*,*,#4618,.T.) ;
#6128 = ORIENTED_EDGE('',*,*,#4619,.T.) ;
#6129 = ORIENTED_EDGE('',*,*,#4620,.T.) ;
#6130 = ORIENTED_EDGE('',*,*,#4621,.T.) ;
#6131 = ORIENTED_EDGE('',*,*,#4622,.T.) ;
#6132 = ORIENTED_EDGE('',*,*,#4623,.T.) ;
#6133 = ORIENTED_EDGE('',*,*,#4624,.T.) ;
#6134 = ORIENTED_EDGE('',*,*,#4625,.T.) ;
#6135 = ORIENTED_EDGE('',*,*,#4626,.T.) ;
#6136 = ORIENTED_EDGE('',*,*,#4627,.T.) ;
#6137 = ORIENTED_EDGE('',*,*,#4628,.T.) ;
#6138 = ORIENTED_EDGE('',*,*,#4629,.T.) ;
#6139 = ORIENTED_EDGE('',*,*,#4630,.T.) ;
#6140 = ORIENTED_EDGE('',*,*,#4631,.T.) ;
#6141 = ORIENTED_EDGE('',*,*,#4632,.T.) ;
#6142 = ORIENTED_EDGE('',*,*,#4633,.T.) ;
#6143 = ORIENTED_EDGE('',*,*,#4634,.T.) ;
#6144 = ORIENTED_EDGE('',*,*,#4635,.T.) ;
#6145 = ORIENTED_EDGE('',*,*,#4636,.F.) ;
#6146 = ORIENTED_EDGE('',*,*,#4637,.T.) ;
#6147 = ORIENTED_EDGE('',*,*,#4638,.F.) ;
#6148 = ORIENTED_EDGE('',*,*,#4639,.F.) ;
#6149 = ORIENTED_EDGE('',*,*,#4518,.F.) ;
#6150 = ORIENTED_EDGE('',*,*,#4640,.F.) ;
#6151 = ORIENTED_EDGE('',*,*,#4637,.F.) ;
#6152 = ORIENTED_EDGE('',*,*,#4636,.T.) ;
#6153 = ORIENTED_EDGE('',*,*,#4639,.T.) ;
#6154 = ORIENTED_EDGE('',*,*,#4641,.T.) ;
#6155 = ORIENTED_EDGE('',*,*,#4642,.F.) ;
#6156 = ORIENTED_EDGE('',*,*,#4520,.F.) ;
#6157 = ORIENTED_EDGE('',*,*,#4643,.F.) ;
#6158 = ORIENTED_EDGE('',*,*,#4641,.F.) ;
#6159 = ORIENTED_EDGE('',*,*,#4638,.T.) ;
#6160 = ORIENTED_EDGE('',*,*,#4640,.T.) ;
#6161 = ORIENTED_EDGE('',*,*,#4519,.F.) ;
#6162 = ORIENTED_EDGE('',*,*,#4642,.T.) ;
#6163 = ORIENTED_EDGE('',*,*,#4643,.T.) ;
#6164 = ORIENTED_EDGE('',*,*,#4522,.F.) ;
#6165 = ORIENTED_EDGE('',*,*,#4644,.T.) ;
#6166 = ORIENTED_EDGE('',*,*,#4523,.F.) ;
#6167 = ORIENTED_EDGE('',*,*,#4645,.F.) ;
#6168 = ORIENTED_EDGE('',*,*,#4524,.F.) ;
#6169 = ORIENTED_EDGE('',*,*,#4644,.F.) ;
#6170 = ORIENTED_EDGE('',*,*,#4521,.F.) ;
#6171 = ORIENTED_EDGE('',*,*,#4645,.T.) ;
#6172 = ORIENTED_EDGE('',*,*,#4526,.F.) ;
#6173 = ORIENTED_EDGE('',*,*,#4646,.T.) ;
#6174 = ORIENTED_EDGE('',*,*,#4527,.F.) ;
#6175 = ORIENTED_EDGE('',*,*,#4647,.F.) ;
#6176 = ORIENTED_EDGE('',*,*,#4528,.F.) ;
#6177 = ORIENTED_EDGE('',*,*,#4646,.F.) ;
#6178 = ORIENTED_EDGE('',*,*,#4525,.F.) ;
#6179 = ORIENTED_EDGE('',*,*,#4647,.T.) ;
#6180 = ORIENTED_EDGE('',*,*,#4530,.F.) ;
#6181 = ORIENTED_EDGE('',*,*,#4648,.T.) ;
#6182 = ORIENTED_EDGE('',*,*,#4531,.F.) ;
#6183 = ORIENTED_EDGE('',*,*,#4649,.F.) ;
#6184 = ORIENTED_EDGE('',*,*,#4532,.F.) ;
#6185 = ORIENTED_EDGE('',*,*,#4648,.F.) ;
#6186 = ORIENTED_EDGE('',*,*,#4529,.F.) ;
#6187 = ORIENTED_EDGE('',*,*,#4649,.T.) ;
#6188 = ORIENTED_EDGE('',*,*,#4534,.F.) ;
#6189 = ORIENTED_EDGE('',*,*,#4650,.T.) ;
#6190 = ORIENTED_EDGE('',*,*,#4535,.F.) ;
#6191 = ORIENTED_EDGE('',*,*,#4651,.F.) ;
#6192 = ORIENTED_EDGE('',*,*,#4652,.F.) ;
#6193 = ORIENTED_EDGE('',*,*,#4536,.F.) ;
#6194 = ORIENTED_EDGE('',*,*,#4650,.F.) ;
#6195 = ORIENTED_EDGE('',*,*,#4533,.F.) ;
#6196 = ORIENTED_EDGE('',*,*,#4652,.T.) ;
#6197 = ORIENTED_EDGE('',*,*,#4653,.T.) ;
#6198 = ORIENTED_EDGE('',*,*,#4654,.F.) ;
#6199 = ORIENTED_EDGE('',*,*,#4655,.F.) ;
#6200 = ORIENTED_EDGE('',*,*,#4538,.F.) ;
#6201 = ORIENTED_EDGE('',*,*,#4656,.F.) ;
#6202 = ORIENTED_EDGE('',*,*,#4653,.F.) ;
#6203 = ORIENTED_EDGE('',*,*,#4651,.T.) ;
#6204 = ORIENTED_EDGE('',*,*,#4537,.F.) ;
#6205 = ORIENTED_EDGE('',*,*,#4655,.T.) ;
#6206 = ORIENTED_EDGE('',*,*,#4657,.T.) ;
#6207 = ORIENTED_EDGE('',*,*,#4658,.F.) ;
#6208 = ORIENTED_EDGE('',*,*,#4540,.F.) ;
#6209 = ORIENTED_EDGE('',*,*,#4659,.F.) ;
#6210 = ORIENTED_EDGE('',*,*,#4657,.F.) ;
#6211 = ORIENTED_EDGE('',*,*,#4654,.T.) ;
#6212 = ORIENTED_EDGE('',*,*,#4656,.T.) ;
#6213 = ORIENTED_EDGE('',*,*,#4539,.F.) ;
#6214 = ORIENTED_EDGE('',*,*,#4658,.T.) ;
#6215 = ORIENTED_EDGE('',*,*,#4660,.T.) ;
#6216 = ORIENTED_EDGE('',*,*,#4661,.F.) ;
#6217 = ORIENTED_EDGE('',*,*,#4662,.F.) ;
#6218 = ORIENTED_EDGE('',*,*,#4542,.F.) ;
#6219 = ORIENTED_EDGE('',*,*,#4663,.F.) ;
#6220 = ORIENTED_EDGE('',*,*,#4660,.F.) ;
#6221 = ORIENTED_EDGE('',*,*,#4659,.T.) ;
#6222 = ORIENTED_EDGE('',*,*,#4541,.F.) ;
#6223 = ORIENTED_EDGE('',*,*,#4662,.T.) ;
#6224 = ORIENTED_EDGE('',*,*,#4664,.T.) ;
#6225 = ORIENTED_EDGE('',*,*,#4665,.F.) ;
#6226 = ORIENTED_EDGE('',*,*,#4544,.F.) ;
#6227 = ORIENTED_EDGE('',*,*,#4666,.F.) ;
#6228 = ORIENTED_EDGE('',*,*,#4664,.F.) ;
#6229 = ORIENTED_EDGE('',*,*,#4661,.T.) ;
#6230 = ORIENTED_EDGE('',*,*,#4663,.T.) ;
#6231 = ORIENTED_EDGE('',*,*,#4543,.F.) ;
#6232 = ORIENTED_EDGE('',*,*,#4665,.T.) ;
#6233 = ORIENTED_EDGE('',*,*,#4666,.T.) ;
#6234 = ORIENTED_EDGE('',*,*,#4546,.F.) ;
#6235 = ORIENTED_EDGE('',*,*,#4667,.T.) ;
#6236 = ORIENTED_EDGE('',*,*,#4547,.F.) ;
#6237 = ORIENTED_EDGE('',*,*,#4668,.F.) ;
#6238 = ORIENTED_EDGE('',*,*,#4548,.F.) ;
#6239 = ORIENTED_EDGE('',*,*,#4667,.F.) ;
#6240 = ORIENTED_EDGE('',*,*,#4545,.F.) ;
#6241 = ORIENTED_EDGE('',*,*,#4668,.T.) ;
#6242 = ORIENTED_EDGE('',*,*,#4550,.F.) ;
#6243 = ORIENTED_EDGE('',*,*,#4669,.T.) ;
#6244 = ORIENTED_EDGE('',*,*,#4551,.F.) ;
#6245 = ORIENTED_EDGE('',*,*,#4670,.F.) ;
#6246 = ORIENTED_EDGE('',*,*,#4552,.F.) ;
#6247 = ORIENTED_EDGE('',*,*,#4669,.F.) ;
#6248 = ORIENTED_EDGE('',*,*,#4549,.F.) ;
#6249 = ORIENTED_EDGE('',*,*,#4670,.T.) ;
#6250 = ORIENTED_EDGE('',*,*,#4554,.F.) ;
#6251 = ORIENTED_EDGE('',*,*,#4671,.T.) ;
#6252 = ORIENTED_EDGE('',*,*,#4555,.F.) ;
#6253 = ORIENTED_EDGE('',*,*,#4672,.F.) ;
#6254 = ORIENTED_EDGE('',*,*,#4556,.F.) ;
#6255 = ORIENTED_EDGE('',*,*,#4671,.F.) ;
#6256 = ORIENTED_EDGE('',*,*,#4553,.F.) ;
#6257 = ORIENTED_EDGE('',*,*,#4672,.T.) ;
#6258 = ORIENTED_EDGE('',*,*,#4558,.F.) ;
#6259 = ORIENTED_EDGE('',*,*,#4673,.T.) ;
#6260 = ORIENTED_EDGE('',*,*,#4559,.F.) ;
#6261 = ORIENTED_EDGE('',*,*,#4674,.F.) ;
#6262 = ORIENTED_EDGE('',*,*,#4675,.F.) ;
#6263 = ORIENTED_EDGE('',*,*,#4560,.F.) ;
#6264 = ORIENTED_EDGE('',*,*,#4673,.F.) ;
#6265 = ORIENTED_EDGE('',*,*,#4557,.F.) ;
#6266 = ORIENTED_EDGE('',*,*,#4675,.T.) ;
#6267 = ORIENTED_EDGE('',*,*,#4676,.T.) ;
#6268 = ORIENTED_EDGE('',*,*,#4677,.F.) ;
#6269 = ORIENTED_EDGE('',*,*,#4678,.F.) ;
#6270 = ORIENTED_EDGE('',*,*,#4562,.F.) ;
#6271 = ORIENTED_EDGE('',*,*,#4679,.F.) ;
#6272 = ORIENTED_EDGE('',*,*,#4676,.F.) ;
#6273 = ORIENTED_EDGE('',*,*,#4674,.T.) ;
#6274 = ORIENTED_EDGE('',*,*,#4561,.F.) ;
#6275 = ORIENTED_EDGE('',*,*,#4678,.T.) ;
#6276 = ORIENTED_EDGE('',*,*,#4680,.T.) ;
#6277 = ORIENTED_EDGE('',*,*,#4681,.F.) ;
#6278 = ORIENTED_EDGE('',*,*,#4564,.F.) ;
#6279 = ORIENTED_EDGE('',*,*,#4682,.F.) ;
#6280 = ORIENTED_EDGE('',*,*,#4680,.F.) ;
#6281 = ORIENTED_EDGE('',*,*,#4677,.T.) ;
#6282 = ORIENTED_EDGE('',*,*,#4679,.T.) ;
#6283 = ORIENTED_EDGE('',*,*,#4563,.F.) ;
#6284 = ORIENTED_EDGE('',*,*,#4681,.T.) ;
#6285 = ORIENTED_EDGE('',*,*,#4683,.T.) ;
#6286 = ORIENTED_EDGE('',*,*,#4684,.F.) ;
#6287 = ORIENTED_EDGE('',*,*,#4685,.F.) ;
#6288 = ORIENTED_EDGE('',*,*,#4566,.F.) ;
#6289 = ORIENTED_EDGE('',*,*,#4686,.F.) ;
#6290 = ORIENTED_EDGE('',*,*,#4683,.F.) ;
#6291 = ORIENTED_EDGE('',*,*,#4682,.T.) ;
#6292 = ORIENTED_EDGE('',*,*,#4565,.F.) ;
#6293 = ORIENTED_EDGE('',*,*,#4685,.T.) ;
#6294 = ORIENTED_EDGE('',*,*,#4687,.T.) ;
#6295 = ORIENTED_EDGE('',*,*,#4688,.F.) ;
#6296 = ORIENTED_EDGE('',*,*,#4568,.F.) ;
#6297 = ORIENTED_EDGE('',*,*,#4689,.F.) ;
#6298 = ORIENTED_EDGE('',*,*,#4687,.F.) ;
#6299 = ORIENTED_EDGE('',*,*,#4684,.T.) ;
#6300 = ORIENTED_EDGE('',*,*,#4686,.T.) ;
#6301 = ORIENTED_EDGE('',*,*,#4567,.F.) ;
#6302 = ORIENTED_EDGE('',*,*,#4688,.T.) ;
#6303 = ORIENTED_EDGE('',*,*,#4689,.T.) ;
#6304 = ORIENTED_EDGE('',*,*,#4570,.F.) ;
#6305 = ORIENTED_EDGE('',*,*,#4690,.T.) ;
#6306 = ORIENTED_EDGE('',*,*,#4571,.F.) ;
#6307 = ORIENTED_EDGE('',*,*,#4691,.F.) ;
#6308 = ORIENTED_EDGE('',*,*,#4572,.F.) ;
#6309 = ORIENTED_EDGE('',*,*,#4690,.F.) ;
#6310 = ORIENTED_EDGE('',*,*,#4569,.F.) ;
#6311 = ORIENTED_EDGE('',*,*,#4691,.T.) ;
#6312 = ORIENTED_EDGE('',*,*,#4574,.F.) ;
#6313 = ORIENTED_EDGE('',*,*,#4692,.T.) ;
#6314 = ORIENTED_EDGE('',*,*,#4575,.F.) ;
#6315 = ORIENTED_EDGE('',*,*,#4693,.F.) ;
#6316 = ORIENTED_EDGE('',*,*,#4576,.F.) ;
#6317 = ORIENTED_EDGE('',*,*,#4692,.F.) ;
#6318 = ORIENTED_EDGE('',*,*,#4573,.F.) ;
#6319 = ORIENTED_EDGE('',*,*,#4693,.T.) ;
#6320 = ORIENTED_EDGE('',*,*,#4578,.F.) ;
#6321 = ORIENTED_EDGE('',*,*,#4694,.T.) ;
#6322 = ORIENTED_EDGE('',*,*,#4579,.F.) ;
#6323 = ORIENTED_EDGE('',*,*,#4695,.F.) ;
#6324 = ORIENTED_EDGE('',*,*,#4580,.F.) ;
#6325 = ORIENTED_EDGE('',*,*,#4694,.F.) ;
#6326 = ORIENTED_EDGE('',*,*,#4577,.F.) ;
#6327 = ORIENTED_EDGE('',*,*,#4695,.T.) ;
#6328 = ORIENTED_EDGE('',*,*,#4582,.F.) ;
#6329 = ORIENTED_EDGE('',*,*,#4696,.T.) ;
#6330 = ORIENTED_EDGE('',*,*,#4583,.F.) ;
#6331 = ORIENTED_EDGE('',*,*,#4697,.F.) ;
#6332 = ORIENTED_EDGE('',*,*,#4698,.F.) ;
#6333 = ORIENTED_EDGE('',*,*,#4584,.F.) ;
#6334 = ORIENTED_EDGE('',*,*,#4696,.F.) ;
#6335 = ORIENTED_EDGE('',*,*,#4581,.F.) ;
#6336 = ORIENTED_EDGE('',*,*,#4698,.T.) ;
#6337 = ORIENTED_EDGE('',*,*,#4699,.T.) ;
#6338 = ORIENTED_EDGE('',*,*,#4700,.F.) ;
#6339 = ORIENTED_EDGE('',*,*,#4701,.F.) ;
#6340 = ORIENTED_EDGE('',*,*,#4586,.F.) ;
#6341 = ORIENTED_EDGE('',*,*,#4702,.F.) ;
#6342 = ORIENTED_EDGE('',*,*,#4699,.F.) ;
#6343 = ORIENTED_EDGE('',*,*,#4697,.T.) ;
#6344 = ORIENTED_EDGE('',*,*,#4585,.F.) ;
#6345 = ORIENTED_EDGE('',*,*,#4701,.T.) ;
#6346 = ORIENTED_EDGE('',*,*,#4703,.T.) ;
#6347 = ORIENTED_EDGE('',*,*,#4704,.F.) ;
#6348 = ORIENTED_EDGE('',*,*,#4588,.F.) ;
#6349 = ORIENTED_EDGE('',*,*,#4705,.F.) ;
#6350 = ORIENTED_EDGE('',*,*,#4703,.F.) ;
#6351 = ORIENTED_EDGE('',*,*,#4700,.T.) ;
#6352 = ORIENTED_EDGE('',*,*,#4702,.T.) ;
#6353 = ORIENTED_EDGE('',*,*,#4587,.F.) ;
#6354 = ORIENTED_EDGE('',*,*,#4704,.T.) ;
#6355 = ORIENTED_EDGE('',*,*,#4706,.T.) ;
#6356 = ORIENTED_EDGE('',*,*,#4707,.F.) ;
#6357 = ORIENTED_EDGE('',*,*,#4708,.F.) ;
#6358 = ORIENTED_EDGE('',*,*,#4590,.F.) ;
#6359 = ORIENTED_EDGE('',*,*,#4709,.F.) ;
#6360 = ORIENTED_EDGE('',*,*,#4706,.F.) ;
#6361 = ORIENTED_EDGE('',*,*,#4705,.T.) ;
#6362 = ORIENTED_EDGE('',*,*,#4589,.F.) ;
#6363 = ORIENTED_EDGE('',*,*,#4708,.T.) ;
#6364 = ORIENTED_EDGE('',*,*,#4710,.T.) ;
#6365 = ORIENTED_EDGE('',*,*,#4711,.F.) ;
#6366 = ORIENTED_EDGE('',*,*,#4592,.F.) ;
#6367 = ORIENTED_EDGE('',*,*,#4712,.F.) ;
#6368 = ORIENTED_EDGE('',*,*,#4710,.F.) ;
#6369 = ORIENTED_EDGE('',*,*,#4707,.T.) ;
#6370 = ORIENTED_EDGE('',*,*,#4709,.T.) ;
#6371 = ORIENTED_EDGE('',*,*,#4591,.F.) ;
#6372 = ORIENTED_EDGE('',*,*,#4711,.T.) ;
#6373 = ORIENTED_EDGE('',*,*,#4712,.T.) ;
#6374 = ORIENTED_EDGE('',*,*,#4594,.F.) ;
#6375 = ORIENTED_EDGE('',*,*,#4713,.T.) ;
#6376 = ORIENTED_EDGE('',*,*,#4595,.F.) ;
#6377 = ORIENTED_EDGE('',*,*,#4714,.F.) ;
#6378 = ORIENTED_EDGE('',*,*,#4596,.F.) ;
#6379 = ORIENTED_EDGE('',*,*,#4713,.F.) ;
#6380 = ORIENTED_EDGE('',*,*,#4593,.F.) ;
#6381 = ORIENTED_EDGE('',*,*,#4714,.T.) ;
#6382 = ORIENTED_EDGE('',*,*,#4598,.F.) ;
#6383 = ORIENTED_EDGE('',*,*,#4715,.T.) ;
#6384 = ORIENTED_EDGE('',*,*,#4599,.F.) ;
#6385 = ORIENTED_EDGE('',*,*,#4716,.F.) ;
#6386 = ORIENTED_EDGE('',*,*,#4600,.F.) ;
#6387 = ORIENTED_EDGE('',*,*,#4715,.F.) ;
#6388 = ORIENTED_EDGE('',*,*,#4597,.F.) ;
#6389 = ORIENTED_EDGE('',*,*,#4716,.T.) ;
#6390 = ORIENTED_EDGE('',*,*,#4602,.F.) ;
#6391 = ORIENTED_EDGE('',*,*,#4717,.T.) ;
#6392 = ORIENTED_EDGE('',*,*,#4603,.F.) ;
#6393 = ORIENTED_EDGE('',*,*,#4718,.F.) ;
#6394 = ORIENTED_EDGE('',*,*,#4604,.F.) ;
#6395 = ORIENTED_EDGE('',*,*,#4717,.F.) ;
#6396 = ORIENTED_EDGE('',*,*,#4601,.F.) ;
#6397 = ORIENTED_EDGE('',*,*,#4718,.T.) ;
#6398 = ORIENTED_EDGE('',*,*,#4606,.F.) ;
#6399 = ORIENTED_EDGE('',*,*,#4719,.T.) ;
#6400 = ORIENTED_EDGE('',*,*,#4607,.F.) ;
#6401 = ORIENTED_EDGE('',*,*,#4720,.F.) ;
#6402 = ORIENTED_EDGE('',*,*,#4721,.F.) ;
#6403 = ORIENTED_EDGE('',*,*,#4608,.F.) ;
#6404 = ORIENTED_EDGE('',*,*,#4719,.F.) ;
#6405 = ORIENTED_EDGE('',*,*,#4605,.F.) ;
#6406 = ORIENTED_EDGE('',*,*,#4721,.T.) ;
#6407 = ORIENTED_EDGE('',*,*,#4722,.T.) ;
#6408 = ORIENTED_EDGE('',*,*,#4723,.F.) ;
#6409 = ORIENTED_EDGE('',*,*,#4724,.F.) ;
#6410 = ORIENTED_EDGE('',*,*,#4610,.F.) ;
#6411 = ORIENTED_EDGE('',*,*,#4725,.F.) ;
#6412 = ORIENTED_EDGE('',*,*,#4722,.F.) ;
#6413 = ORIENTED_EDGE('',*,*,#4720,.T.) ;
#6414 = ORIENTED_EDGE('',*,*,#4609,.F.) ;
#6415 = ORIENTED_EDGE('',*,*,#4724,.T.) ;
#6416 = ORIENTED_EDGE('',*,*,#4726,.T.) ;
#6417 = ORIENTED_EDGE('',*,*,#4727,.F.) ;
#6418 = ORIENTED_EDGE('',*,*,#4612,.F.) ;
#6419 = ORIENTED_EDGE('',*,*,#4728,.F.) ;
#6420 = ORIENTED_EDGE('',*,*,#4726,.F.) ;
#6421 = ORIENTED_EDGE('',*,*,#4723,.T.) ;
#6422 = ORIENTED_EDGE('',*,*,#4725,.T.) ;
#6423 = ORIENTED_EDGE('',*,*,#4611,.F.) ;
#6424 = ORIENTED_EDGE('',*,*,#4727,.T.) ;
#6425 = ORIENTED_EDGE('',*,*,#4729,.T.) ;
#6426 = ORIENTED_EDGE('',*,*,#4730,.F.) ;
#6427 = ORIENTED_EDGE('',*,*,#4731,.F.) ;
#6428 = ORIENTED_EDGE('',*,*,#4614,.F.) ;
#6429 = ORIENTED_EDGE('',*,*,#4732,.F.) ;
#6430 = ORIENTED_EDGE('',*,*,#4729,.F.) ;
#6431 = ORIENTED_EDGE('',*,*,#4728,.T.) ;
#6432 = ORIENTED_EDGE('',*,*,#4613,.F.) ;
#6433 = ORIENTED_EDGE('',*,*,#4731,.T.) ;
#6434 = ORIENTED_EDGE('',*,*,#4733,.T.) ;
#6435 = ORIENTED_EDGE('',*,*,#4734,.F.) ;
#6436 = ORIENTED_EDGE('',*,*,#4616,.F.) ;
#6437 = ORIENTED_EDGE('',*,*,#4735,.F.) ;
#6438 = ORIENTED_EDGE('',*,*,#4733,.F.) ;
#6439 = ORIENTED_EDGE('',*,*,#4730,.T.) ;
#6440 = ORIENTED_EDGE('',*,*,#4732,.T.) ;
#6441 = ORIENTED_EDGE('',*,*,#4615,.F.) ;
#6442 = ORIENTED_EDGE('',*,*,#4734,.T.) ;
#6443 = ORIENTED_EDGE('',*,*,#4735,.T.) ;
#6444 = ORIENTED_EDGE('',*,*,#4618,.F.) ;
#6445 = ORIENTED_EDGE('',*,*,#4736,.T.) ;
#6446 = ORIENTED_EDGE('',*,*,#4619,.F.) ;
#6447 = ORIENTED_EDGE('',*,*,#4737,.F.) ;
#6448 = ORIENTED_EDGE('',*,*,#4620,.F.) ;
#6449 = ORIENTED_EDGE('',*,*,#4736,.F.) ;
#6450 = ORIENTED_EDGE('',*,*,#4617,.F.) ;
#6451 = ORIENTED_EDGE('',*,*,#4737,.T.) ;
#6452 = ORIENTED_EDGE('',*,*,#4622,.F.) ;
#6453 = ORIENTED_EDGE('',*,*,#4738,.T.) ;
#6454 = ORIENTED_EDGE('',*,*,#4623,.F.) ;
#6455 = ORIENTED_EDGE('',*,*,#4739,.F.) ;
#6456 = ORIENTED_EDGE('',*,*,#4624,.F.) ;
#6457 = ORIENTED_EDGE('',*,*,#4738,.F.) ;
#6458 = ORIENTED_EDGE('',*,*,#4621,.F.) ;
#6459 = ORIENTED_EDGE('',*,*,#4739,.T.) ;
#6460 = ORIENTED_EDGE('',*,*,#4626,.F.) ;
#6461 = ORIENTED_EDGE('',*,*,#4740,.T.) ;
#6462 = ORIENTED_EDGE('',*,*,#4627,.F.) ;
#6463 = ORIENTED_EDGE('',*,*,#4741,.F.) ;
#6464 = ORIENTED_EDGE('',*,*,#4628,.F.) ;
#6465 = ORIENTED_EDGE('',*,*,#4740,.F.) ;
#6466 = ORIENTED_EDGE('',*,*,#4625,.F.) ;
#6467 = ORIENTED_EDGE('',*,*,#4741,.T.) ;
#6468 = ORIENTED_EDGE('',*,*,#4630,.F.) ;
#6469 = ORIENTED_EDGE('',*,*,#4742,.T.) ;
#6470 = ORIENTED_EDGE('',*,*,#4631,.F.) ;
#6471 = ORIENTED_EDGE('',*,*,#4743,.F.) ;
#6472 = ORIENTED_EDGE('',*,*,#4744,.F.) ;
#6473 = ORIENTED_EDGE('',*,*,#4632,.F.) ;
#6474 = ORIENTED_EDGE('',*,*,#4742,.F.) ;
#6475 = ORIENTED_EDGE('',*,*,#4629,.F.) ;
#6476 = ORIENTED_EDGE('',*,*,#4744,.T.) ;
#6477 = ORIENTED_EDGE('',*,*,#4745,.T.) ;
#6478 = ORIENTED_EDGE('',*,*,#4746,.F.) ;
#6479 = ORIENTED_EDGE('',*,*,#4747,.F.) ;
#6480 = ORIENTED_EDGE('',*,*,#4634,.F.) ;
#6481 = ORIENTED_EDGE('',*,*,#4748,.F.) ;
#6482 = ORIENTED_EDGE('',*,*,#4745,.F.) ;
#6483 = ORIENTED_EDGE('',*,*,#4743,.T.) ;
#6484 = ORIENTED_EDGE('',*,*,#4633,.F.) ;
#6485 = ORIENTED_EDGE('',*,*,#4747,.T.) ;
#6486 = ORIENTED_EDGE('',*,*,#4749,.T.) ;
#6487 = ORIENTED_EDGE('',*,*,#4750,.F.) ;
#6488 = ORIENTED_EDGE('',*,*,#4749,.F.) ;
#6489 = ORIENTED_EDGE('',*,*,#4746,.T.) ;
#6490 = ORIENTED_EDGE('',*,*,#4748,.T.) ;
#6491 = ORIENTED_EDGE('',*,*,#4635,.F.) ;
#6492 = ORIENTED_EDGE('',*,*,#4750,.T.) ;
#6493 = ORIENTED_EDGE('',*,*,#4751,.T.) ;
#6494 = ORIENTED_EDGE('',*,*,#4752,.F.) ;
#6495 = ORIENTED_EDGE('',*,*,#4753,.T.) ;
#6496 = ORIENTED_EDGE('',*,*,#4754,.F.) ;
#6497 = ORIENTED_EDGE('',*,*,#4753,.F.) ;
#6498 = ORIENTED_EDGE('',*,*,#4755,.T.) ;
#6499 = ORIENTED_EDGE('',*,*,#4751,.F.) ;
#6500 = ORIENTED_EDGE('',*,*,#4755,.F.) ;
#6501 = ORIENTED_EDGE('',*,*,#4756,.F.) ;
#6502 = ORIENTED_EDGE('',*,*,#4757,.T.) ;
#6503 = ORIENTED_EDGE('',*,*,#4754,.T.) ;
#6504 = ORIENTED_EDGE('',*,*,#4757,.F.) ;
#6505 = ORIENTED_EDGE('',*,*,#4752,.T.) ;
#6506 = ORIENTED_EDGE('',*,*,#4758,.T.) ;
#6507 = ORIENTED_EDGE('',*,*,#4759,.F.) ;
#6508 = ORIENTED_EDGE('',*,*,#4758,.F.) ;
#6509 = ORIENTED_EDGE('',*,*,#4759,.T.) ;
#6510 = ORIENTED_EDGE('',*,*,#4756,.T.) ;
#6511 = ORIENTED_EDGE('',*,*,#4760,.T.) ;
#6512 = ORIENTED_EDGE('',*,*,#4761,.T.) ;
#6513 = ORIENTED_EDGE('',*,*,#4762,.T.) ;
#6514 = ORIENTED_EDGE('',*,*,#4763,.T.) ;
#6515 = ORIENTED_EDGE('',*,*,#4764,.T.) ;
#6516 = ORIENTED_EDGE('',*,*,#4765,.F.) ;
#6517 = ORIENTED_EDGE('',*,*,#4766,.F.) ;
#6518 = ORIENTED_EDGE('',*,*,#4763,.F.) ;
#6519 = ORIENTED_EDGE('',*,*,#4767,.T.) ;
#6520 = ORIENTED_EDGE('',*,*,#4768,.F.) ;
#6521 = ORIENTED_EDGE('',*,*,#4764,.F.) ;
#6522 = ORIENTED_EDGE('',*,*,#4762,.F.) ;
#6523 = ORIENTED_EDGE('',*,*,#4769,.T.) ;
#6524 = ORIENTED_EDGE('',*,*,#4770,.F.) ;
#6525 = ORIENTED_EDGE('',*,*,#4767,.F.) ;
#6526 = ORIENTED_EDGE('',*,*,#4761,.F.) ;
#6527 = ORIENTED_EDGE('',*,*,#4766,.T.) ;
#6528 = ORIENTED_EDGE('',*,*,#4771,.F.) ;
#6529 = ORIENTED_EDGE('',*,*,#4769,.F.) ;
#6530 = ORIENTED_EDGE('',*,*,#4760,.F.) ;
#6531 = ORIENTED_EDGE('',*,*,#4772,.F.) ;
#6532 = ORIENTED_EDGE('',*,*,#4773,.T.) ;
#6533 = ORIENTED_EDGE('',*,*,#4774,.T.) ;
#6534 = ORIENTED_EDGE('',*,*,#4773,.F.) ;
#6535 = ORIENTED_EDGE('',*,*,#4774,.F.) ;
#6536 = ORIENTED_EDGE('',*,*,#4775,.T.) ;
#6537 = ORIENTED_EDGE('',*,*,#4776,.T.) ;
#6538 = ORIENTED_EDGE('',*,*,#4777,.T.) ;
#6539 = ORIENTED_EDGE('',*,*,#4778,.T.) ;
#6540 = ORIENTED_EDGE('',*,*,#4765,.T.) ;
#6541 = ORIENTED_EDGE('',*,*,#4768,.T.) ;
#6542 = ORIENTED_EDGE('',*,*,#4770,.T.) ;
#6543 = ORIENTED_EDGE('',*,*,#4771,.T.) ;
#6544 = ORIENTED_EDGE('',*,*,#4779,.T.) ;
#6545 = ORIENTED_EDGE('',*,*,#4780,.T.) ;
#6546 = ORIENTED_EDGE('',*,*,#4781,.T.) ;
#6547 = ORIENTED_EDGE('',*,*,#4782,.T.) ;
#6548 = ORIENTED_EDGE('',*,*,#4772,.T.) ;
#6549 = ORIENTED_EDGE('',*,*,#4783,.T.) ;
#6550 = ORIENTED_EDGE('',*,*,#4780,.F.) ;
#6551 = ORIENTED_EDGE('',*,*,#4784,.F.) ;
#6552 = ORIENTED_EDGE('',*,*,#4778,.F.) ;
#6553 = ORIENTED_EDGE('',*,*,#4785,.T.) ;
#6554 = ORIENTED_EDGE('',*,*,#4781,.F.) ;
#6555 = ORIENTED_EDGE('',*,*,#4783,.F.) ;
#6556 = ORIENTED_EDGE('',*,*,#4777,.F.) ;
#6557 = ORIENTED_EDGE('',*,*,#4786,.T.) ;
#6558 = ORIENTED_EDGE('',*,*,#4782,.F.) ;
#6559 = ORIENTED_EDGE('',*,*,#4785,.F.) ;
#6560 = ORIENTED_EDGE('',*,*,#4776,.F.) ;
#6561 = ORIENTED_EDGE('',*,*,#4784,.T.) ;
#6562 = ORIENTED_EDGE('',*,*,#4779,.F.) ;
#6563 = ORIENTED_EDGE('',*,*,#4786,.F.) ;
#6564 = ORIENTED_EDGE('',*,*,#4775,.F.) ;
#6565 = ORIENTED_EDGE('',*,*,#4787,.T.) ;
#6566 = ORIENTED_EDGE('',*,*,#4788,.T.) ;
#6567 = ORIENTED_EDGE('',*,*,#4789,.T.) ;
#6568 = ORIENTED_EDGE('',*,*,#4790,.T.) ;
#6569 = ORIENTED_EDGE('',*,*,#4791,.T.) ;
#6570 = ORIENTED_EDGE('',*,*,#4792,.T.) ;
#6571 = ORIENTED_EDGE('',*,*,#4793,.T.) ;
#6572 = ORIENTED_EDGE('',*,*,#4794,.T.) ;
#6573 = ORIENTED_EDGE('',*,*,#4795,.T.) ;
#6574 = ORIENTED_EDGE('',*,*,#4796,.T.) ;
#6575 = ORIENTED_EDGE('',*,*,#4797,.T.) ;
#6576 = ORIENTED_EDGE('',*,*,#4798,.T.) ;
#6577 = ORIENTED_EDGE('',*,*,#4799,.T.) ;
#6578 = ORIENTED_EDGE('',*,*,#4800,.T.) ;
#6579 = ORIENTED_EDGE('',*,*,#4801,.T.) ;
#6580 = ORIENTED_EDGE('',*,*,#4802,.T.) ;
#6581 = ORIENTED_EDGE('',*,*,#4803,.T.) ;
#6582 = ORIENTED_EDGE('',*,*,#4804,.T.) ;
#6583 = ORIENTED_EDGE('',*,*,#4805,.T.) ;
#6584 = ORIENTED_EDGE('',*,*,#4806,.T.) ;
#6585 = ORIENTED_EDGE('',*,*,#4807,.T.) ;
#6586 = ORIENTED_EDGE('',*,*,#4808,.T.) ;
#6587 = ORIENTED_EDGE('',*,*,#4809,.T.) ;
#6588 = ORIENTED_EDGE('',*,*,#4810,.T.) ;
#6589 = ORIENTED_EDGE('',*,*,#4811,.T.) ;
#6590 = ORIENTED_EDGE('',*,*,#4812,.T.) ;
#6591 = ORIENTED_EDGE('',*,*,#4813,.T.) ;
#6592 = ORIENTED_EDGE('',*,*,#4814,.T.) ;
#6593 = ORIENTED_EDGE('',*,*,#4815,.T.) ;
#6594 = ORIENTED_EDGE('',*,*,#4816,.T.) ;
#6595 = ORIENTED_EDGE('',*,*,#4817,.T.) ;
#6596 = ORIENTED_EDGE('',*,*,#4818,.T.) ;
#6597 = ORIENTED_EDGE('',*,*,#4819,.T.) ;
#6598 = ORIENTED_EDGE('',*,*,#4820,.T.) ;
#6599 = ORIENTED_EDGE('',*,*,#4821,.T.) ;
#6600 = ORIENTED_EDGE('',*,*,#4822,.T.) ;
#6601 = ORIENTED_EDGE('',*,*,#4823,.T.) ;
#6602 = ORIENTED_EDGE('',*,*,#4824,.T.) ;
#6603 = ORIENTED_EDGE('',*,*,#4825,.T.) ;
#6604 = ORIENTED_EDGE('',*,*,#4826,.T.) ;
#6605 = ORIENTED_EDGE('',*,*,#4827,.T.) ;
#6606 = ORIENTED_EDGE('',*,*,#4828,.T.) ;
#6607 = ORIENTED_EDGE('',*,*,#4829,.T.) ;
#6608 = ORIENTED_EDGE('',*,*,#4830,.T.) ;
#6609 = ORIENTED_EDGE('',*,*,#4831,.T.) ;
#6610 = ORIENTED_EDGE('',*,*,#4832,.T.) ;
#6611 = ORIENTED_EDGE('',*,*,#4833,.T.) ;
#6612 = ORIENTED_EDGE('',*,*,#4834,.T.) ;
#6613 = ORIENTED_EDGE('',*,*,#4835,.T.) ;
#6614 = ORIENTED_EDGE('',*,*,#4836,.T.) ;
#6615 = ORIENTED_EDGE('',*,*,#4837,.T.) ;
#6616 = ORIENTED_EDGE('',*,*,#4838,.T.) ;
#6617 = ORIENTED_EDGE('',*,*,#4839,.T.) ;
#6618 = ORIENTED_EDGE('',*,*,#4840,.T.) ;
#6619 = ORIENTED_EDGE('',*,*,#4841,.T.) ;
#6620 = ORIENTED_EDGE('',*,*,#4842,.T.) ;
#6621 = ORIENTED_EDGE('',*,*,#4843,.T.) ;
#6622 = ORIENTED_EDGE('',*,*,#4844,.T.) ;
#6623 = ORIENTED_EDGE('',*,*,#4845,.T.) ;
#6624 = ORIENTED_EDGE('',*,*,#4846,.T.) ;
#6625 = ORIENTED_EDGE('',*,*,#4847,.T.) ;
#6626 = ORIENTED_EDGE('',*,*,#4848,.T.) ;
#6627 = ORIENTED_EDGE('',*,*,#4849,.T.) ;
#6628 = ORIENTED_EDGE('',*,*,#4850,.T.) ;
#6629 = ORIENTED_EDGE('',*,*,#4851,.T.) ;
#6630 = ORIENTED_EDGE('',*,*,#4852,.T.) ;
#6631 = ORIENTED_EDGE('',*,*,#4853,.T.) ;
#6632 = ORIENTED_EDGE('',*,*,#4854,.T.) ;
#6633 = ORIENTED_EDGE('',*,*,#4855,.T.) ;
#6634 = ORIENTED_EDGE('',*,*,#4856,.T.) ;
#6635 = ORIENTED_EDGE('',*,*,#4857,.F.) ;
#6636 = ORIENTED_EDGE('',*,*,#4858,.T.) ;
#6637 = ORIENTED_EDGE('',*,*,#4859,.F.) ;
#6638 = ORIENTED_EDGE('',*,*,#4860,.F.) ;
#6639 = ORIENTED_EDGE('',*,*,#4787,.F.) ;
#6640 = ORIENTED_EDGE('',*,*,#4861,.F.) ;
#6641 = ORIENTED_EDGE('',*,*,#4858,.F.) ;
#6642 = ORIENTED_EDGE('',*,*,#4857,.T.) ;
#6643 = ORIENTED_EDGE('',*,*,#4860,.T.) ;
#6644 = ORIENTED_EDGE('',*,*,#4862,.T.) ;
#6645 = ORIENTED_EDGE('',*,*,#4863,.F.) ;
#6646 = ORIENTED_EDGE('',*,*,#4789,.F.) ;
#6647 = ORIENTED_EDGE('',*,*,#4864,.F.) ;
#6648 = ORIENTED_EDGE('',*,*,#4862,.F.) ;
#6649 = ORIENTED_EDGE('',*,*,#4859,.T.) ;
#6650 = ORIENTED_EDGE('',*,*,#4861,.T.) ;
#6651 = ORIENTED_EDGE('',*,*,#4788,.F.) ;
#6652 = ORIENTED_EDGE('',*,*,#4863,.T.) ;
#6653 = ORIENTED_EDGE('',*,*,#4864,.T.) ;
#6654 = ORIENTED_EDGE('',*,*,#4791,.F.) ;
#6655 = ORIENTED_EDGE('',*,*,#4865,.T.) ;
#6656 = ORIENTED_EDGE('',*,*,#4792,.F.) ;
#6657 = ORIENTED_EDGE('',*,*,#4866,.F.) ;
#6658 = ORIENTED_EDGE('',*,*,#4793,.F.) ;
#6659 = ORIENTED_EDGE('',*,*,#4865,.F.) ;
#6660 = ORIENTED_EDGE('',*,*,#4790,.F.) ;
#6661 = ORIENTED_EDGE('',*,*,#4866,.T.) ;
#6662 = ORIENTED_EDGE('',*,*,#4795,.F.) ;
#6663 = ORIENTED_EDGE('',*,*,#4867,.T.) ;
#6664 = ORIENTED_EDGE('',*,*,#4796,.F.) ;
#6665 = ORIENTED_EDGE('',*,*,#4868,.F.) ;
#6666 = ORIENTED_EDGE('',*,*,#4797,.F.) ;
#6667 = ORIENTED_EDGE('',*,*,#4867,.F.) ;
#6668 = ORIENTED_EDGE('',*,*,#4794,.F.) ;
#6669 = ORIENTED_EDGE('',*,*,#4868,.T.) ;
#6670 = ORIENTED_EDGE('',*,*,#4799,.F.) ;
#6671 = ORIENTED_EDGE('',*,*,#4869,.T.) ;
#6672 = ORIENTED_EDGE('',*,*,#4800,.F.) ;
#6673 = ORIENTED_EDGE('',*,*,#4870,.F.) ;
#6674 = ORIENTED_EDGE('',*,*,#4801,.F.) ;
#6675 = ORIENTED_EDGE('',*,*,#4869,.F.) ;
#6676 = ORIENTED_EDGE('',*,*,#4798,.F.) ;
#6677 = ORIENTED_EDGE('',*,*,#4870,.T.) ;
#6678 = ORIENTED_EDGE('',*,*,#4803,.F.) ;
#6679 = ORIENTED_EDGE('',*,*,#4871,.T.) ;
#6680 = ORIENTED_EDGE('',*,*,#4804,.F.) ;
#6681 = ORIENTED_EDGE('',*,*,#4872,.F.) ;
#6682 = ORIENTED_EDGE('',*,*,#4873,.F.) ;
#6683 = ORIENTED_EDGE('',*,*,#4805,.F.) ;
#6684 = ORIENTED_EDGE('',*,*,#4871,.F.) ;
#6685 = ORIENTED_EDGE('',*,*,#4802,.F.) ;
#6686 = ORIENTED_EDGE('',*,*,#4873,.T.) ;
#6687 = ORIENTED_EDGE('',*,*,#4874,.T.) ;
#6688 = ORIENTED_EDGE('',*,*,#4875,.F.) ;
#6689 = ORIENTED_EDGE('',*,*,#4876,.F.) ;
#6690 = ORIENTED_EDGE('',*,*,#4807,.F.) ;
#6691 = ORIENTED_EDGE('',*,*,#4877,.F.) ;
#6692 = ORIENTED_EDGE('',*,*,#4874,.F.) ;
#6693 = ORIENTED_EDGE('',*,*,#4872,.T.) ;
#6694 = ORIENTED_EDGE('',*,*,#4806,.F.) ;
#6695 = ORIENTED_EDGE('',*,*,#4876,.T.) ;
#6696 = ORIENTED_EDGE('',*,*,#4878,.T.) ;
#6697 = ORIENTED_EDGE('',*,*,#4879,.F.) ;
#6698 = ORIENTED_EDGE('',*,*,#4809,.F.) ;
#6699 = ORIENTED_EDGE('',*,*,#4880,.F.) ;
#6700 = ORIENTED_EDGE('',*,*,#4878,.F.) ;
#6701 = ORIENTED_EDGE('',*,*,#4875,.T.) ;
#6702 = ORIENTED_EDGE('',*,*,#4877,.T.) ;
#6703 = ORIENTED_EDGE('',*,*,#4808,.F.) ;
#6704 = ORIENTED_EDGE('',*,*,#4879,.T.) ;
#6705 = ORIENTED_EDGE('',*,*,#4881,.T.) ;
#6706 = ORIENTED_EDGE('',*,*,#4882,.F.) ;
#6707 = ORIENTED_EDGE('',*,*,#4883,.F.) ;
#6708 = ORIENTED_EDGE('',*,*,#4811,.F.) ;
#6709 = ORIENTED_EDGE('',*,*,#4884,.F.) ;
#6710 = ORIENTED_EDGE('',*,*,#4881,.F.) ;
#6711 = ORIENTED_EDGE('',*,*,#4880,.T.) ;
#6712 = ORIENTED_EDGE('',*,*,#4810,.F.) ;
#6713 = ORIENTED_EDGE('',*,*,#4883,.T.) ;
#6714 = ORIENTED_EDGE('',*,*,#4885,.T.) ;
#6715 = ORIENTED_EDGE('',*,*,#4886,.F.) ;
#6716 = ORIENTED_EDGE('',*,*,#4813,.F.) ;
#6717 = ORIENTED_EDGE('',*,*,#4887,.F.) ;
#6718 = ORIENTED_EDGE('',*,*,#4885,.F.) ;
#6719 = ORIENTED_EDGE('',*,*,#4882,.T.) ;
#6720 = ORIENTED_EDGE('',*,*,#4884,.T.) ;
#6721 = ORIENTED_EDGE('',*,*,#4812,.F.) ;
#6722 = ORIENTED_EDGE('',*,*,#4886,.T.) ;
#6723 = ORIENTED_EDGE('',*,*,#4887,.T.) ;
#6724 = ORIENTED_EDGE('',*,*,#4815,.F.) ;
#6725 = ORIENTED_EDGE('',*,*,#4888,.T.) ;
#6726 = ORIENTED_EDGE('',*,*,#4816,.F.) ;
#6727 = ORIENTED_EDGE('',*,*,#4889,.F.) ;
#6728 = ORIENTED_EDGE('',*,*,#4817,.F.) ;
#6729 = ORIENTED_EDGE('',*,*,#4888,.F.) ;
#6730 = ORIENTED_EDGE('',*,*,#4814,.F.) ;
#6731 = ORIENTED_EDGE('',*,*,#4889,.T.) ;
#6732 = ORIENTED_EDGE('',*,*,#4819,.F.) ;
#6733 = ORIENTED_EDGE('',*,*,#4890,.T.) ;
#6734 = ORIENTED_EDGE('',*,*,#4820,.F.) ;
#6735 = ORIENTED_EDGE('',*,*,#4891,.F.) ;
#6736 = ORIENTED_EDGE('',*,*,#4821,.F.) ;
#6737 = ORIENTED_EDGE('',*,*,#4890,.F.) ;
#6738 = ORIENTED_EDGE('',*,*,#4818,.F.) ;
#6739 = ORIENTED_EDGE('',*,*,#4891,.T.) ;
#6740 = ORIENTED_EDGE('',*,*,#4823,.F.) ;
#6741 = ORIENTED_EDGE('',*,*,#4892,.T.) ;
#6742 = ORIENTED_EDGE('',*,*,#4824,.F.) ;
#6743 = ORIENTED_EDGE('',*,*,#4893,.F.) ;
#6744 = ORIENTED_EDGE('',*,*,#4825,.F.) ;
#6745 = ORIENTED_EDGE('',*,*,#4892,.F.) ;
#6746 = ORIENTED_EDGE('',*,*,#4822,.F.) ;
#6747 = ORIENTED_EDGE('',*,*,#4893,.T.) ;
#6748 = ORIENTED_EDGE('',*,*,#4827,.F.) ;
#6749 = ORIENTED_EDGE('',*,*,#4894,.T.) ;
#6750 = ORIENTED_EDGE('',*,*,#4828,.F.) ;
#6751 = ORIENTED_EDGE('',*,*,#4895,.F.) ;
#6752 = ORIENTED_EDGE('',*,*,#4896,.F.) ;
#6753 = ORIENTED_EDGE('',*,*,#4829,.F.) ;
#6754 = ORIENTED_EDGE('',*,*,#4894,.F.) ;
#6755 = ORIENTED_EDGE('',*,*,#4826,.F.) ;
#6756 = ORIENTED_EDGE('',*,*,#4896,.T.) ;
#6757 = ORIENTED_EDGE('',*,*,#4897,.T.) ;
#6758 = ORIENTED_EDGE('',*,*,#4898,.F.) ;
#6759 = ORIENTED_EDGE('',*,*,#4899,.F.) ;
#6760 = ORIENTED_EDGE('',*,*,#4831,.F.) ;
#6761 = ORIENTED_EDGE('',*,*,#4900,.F.) ;
#6762 = ORIENTED_EDGE('',*,*,#4897,.F.) ;
#6763 = ORIENTED_EDGE('',*,*,#4895,.T.) ;
#6764 = ORIENTED_EDGE('',*,*,#4830,.F.) ;
#6765 = ORIENTED_EDGE('',*,*,#4899,.T.) ;
#6766 = ORIENTED_EDGE('',*,*,#4901,.T.) ;
#6767 = ORIENTED_EDGE('',*,*,#4902,.F.) ;
#6768 = ORIENTED_EDGE('',*,*,#4833,.F.) ;
#6769 = ORIENTED_EDGE('',*,*,#4903,.F.) ;
#6770 = ORIENTED_EDGE('',*,*,#4901,.F.) ;
#6771 = ORIENTED_EDGE('',*,*,#4898,.T.) ;
#6772 = ORIENTED_EDGE('',*,*,#4900,.T.) ;
#6773 = ORIENTED_EDGE('',*,*,#4832,.F.) ;
#6774 = ORIENTED_EDGE('',*,*,#4902,.T.) ;
#6775 = ORIENTED_EDGE('',*,*,#4904,.T.) ;
#6776 = ORIENTED_EDGE('',*,*,#4905,.F.) ;
#6777 = ORIENTED_EDGE('',*,*,#4906,.F.) ;
#6778 = ORIENTED_EDGE('',*,*,#4835,.F.) ;
#6779 = ORIENTED_EDGE('',*,*,#4907,.F.) ;
#6780 = ORIENTED_EDGE('',*,*,#4904,.F.) ;
#6781 = ORIENTED_EDGE('',*,*,#4903,.T.) ;
#6782 = ORIENTED_EDGE('',*,*,#4834,.F.) ;
#6783 = ORIENTED_EDGE('',*,*,#4906,.T.) ;
#6784 = ORIENTED_EDGE('',*,*,#4908,.T.) ;
#6785 = ORIENTED_EDGE('',*,*,#4909,.F.) ;
#6786 = ORIENTED_EDGE('',*,*,#4837,.F.) ;
#6787 = ORIENTED_EDGE('',*,*,#4910,.F.) ;
#6788 = ORIENTED_EDGE('',*,*,#4908,.F.) ;
#6789 = ORIENTED_EDGE('',*,*,#4905,.T.) ;
#6790 = ORIENTED_EDGE('',*,*,#4907,.T.) ;
#6791 = ORIENTED_EDGE('',*,*,#4836,.F.) ;
#6792 = ORIENTED_EDGE('',*,*,#4909,.T.) ;
#6793 = ORIENTED_EDGE('',*,*,#4910,.T.) ;
#6794 = ORIENTED_EDGE('',*,*,#4839,.F.) ;
#6795 = ORIENTED_EDGE('',*,*,#4911,.T.) ;
#6796 = ORIENTED_EDGE('',*,*,#4840,.F.) ;
#6797 = ORIENTED_EDGE('',*,*,#4912,.F.) ;
#6798 = ORIENTED_EDGE('',*,*,#4841,.F.) ;
#6799 = ORIENTED_EDGE('',*,*,#4911,.F.) ;
#6800 = ORIENTED_EDGE('',*,*,#4838,.F.) ;
#6801 = ORIENTED_EDGE('',*,*,#4912,.T.) ;
#6802 = ORIENTED_EDGE('',*,*,#4843,.F.) ;
#6803 = ORIENTED_EDGE('',*,*,#4913,.T.) ;
#6804 = ORIENTED_EDGE('',*,*,#4844,.F.) ;
#6805 = ORIENTED_EDGE('',*,*,#4914,.F.) ;
#6806 = ORIENTED_EDGE('',*,*,#4845,.F.) ;
#6807 = ORIENTED_EDGE('',*,*,#4913,.F.) ;
#6808 = ORIENTED_EDGE('',*,*,#4842,.F.) ;
#6809 = ORIENTED_EDGE('',*,*,#4914,.T.) ;
#6810 = ORIENTED_EDGE('',*,*,#4847,.F.) ;
#6811 = ORIENTED_EDGE('',*,*,#4915,.T.) ;
#6812 = ORIENTED_EDGE('',*,*,#4848,.F.) ;
#6813 = ORIENTED_EDGE('',*,*,#4916,.F.) ;
#6814 = ORIENTED_EDGE('',*,*,#4849,.F.) ;
#6815 = ORIENTED_EDGE('',*,*,#4915,.F.) ;
#6816 = ORIENTED_EDGE('',*,*,#4846,.F.) ;
#6817 = ORIENTED_EDGE('',*,*,#4916,.T.) ;
#6818 = ORIENTED_EDGE('',*,*,#4851,.F.) ;
#6819 = ORIENTED_EDGE('',*,*,#4917,.T.) ;
#6820 = ORIENTED_EDGE('',*,*,#4852,.F.) ;
#6821 = ORIENTED_EDGE('',*,*,#4918,.F.) ;
#6822 = ORIENTED_EDGE('',*,*,#4919,.F.) ;
#6823 = ORIENTED_EDGE('',*,*,#4853,.F.) ;
#6824 = ORIENTED_EDGE('',*,*,#4917,.F.) ;
#6825 = ORIENTED_EDGE('',*,*,#4850,.F.) ;
#6826 = ORIENTED_EDGE('',*,*,#4919,.T.) ;
#6827 = ORIENTED_EDGE('',*,*,#4920,.T.) ;
#6828 = ORIENTED_EDGE('',*,*,#4921,.F.) ;
#6829 = ORIENTED_EDGE('',*,*,#4922,.F.) ;
#6830 = ORIENTED_EDGE('',*,*,#4855,.F.) ;
#6831 = ORIENTED_EDGE('',*,*,#4923,.F.) ;
#6832 = ORIENTED_EDGE('',*,*,#4920,.F.) ;
#6833 = ORIENTED_EDGE('',*,*,#4918,.T.) ;
#6834 = ORIENTED_EDGE('',*,*,#4854,.F.) ;
#6835 = ORIENTED_EDGE('',*,*,#4922,.T.) ;
#6836 = ORIENTED_EDGE('',*,*,#4924,.T.) ;
#6837 = ORIENTED_EDGE('',*,*,#4925,.F.) ;
#6838 = ORIENTED_EDGE('',*,*,#4924,.F.) ;
#6839 = ORIENTED_EDGE('',*,*,#4921,.T.) ;
#6840 = ORIENTED_EDGE('',*,*,#4923,.T.) ;
#6841 = ORIENTED_EDGE('',*,*,#4856,.F.) ;
#6842 = ORIENTED_EDGE('',*,*,#4925,.T.) ;
#6843 = ORIENTED_EDGE('',*,*,#4926,.F.) ;
#6844 = ORIENTED_EDGE('',*,*,#4927,.T.) ;
#6845 = ORIENTED_EDGE('',*,*,#4928,.F.) ;
#6846 = ORIENTED_EDGE('',*,*,#4927,.F.) ;
#6847 = ORIENTED_EDGE('',*,*,#4926,.T.) ;
#6848 = ORIENTED_EDGE('',*,*,#4929,.T.) ;
#6849 = ORIENTED_EDGE('',*,*,#4930,.T.) ;
#6850 = ORIENTED_EDGE('',*,*,#4931,.T.) ;
#6851 = ORIENTED_EDGE('',*,*,#4932,.T.) ;
#6852 = ORIENTED_EDGE('',*,*,#4928,.T.) ;
#6853 = ORIENTED_EDGE('',*,*,#4933,.T.) ;
#6854 = ORIENTED_EDGE('',*,*,#4934,.T.) ;
#6855 = ORIENTED_EDGE('',*,*,#4935,.T.) ;
#6856 = ORIENTED_EDGE('',*,*,#4936,.T.) ;
#6857 = ORIENTED_EDGE('',*,*,#4937,.T.) ;
#6858 = ORIENTED_EDGE('',*,*,#4934,.F.) ;
#6859 = ORIENTED_EDGE('',*,*,#4938,.F.) ;
#6860 = ORIENTED_EDGE('',*,*,#4932,.F.) ;
#6861 = ORIENTED_EDGE('',*,*,#4939,.T.) ;
#6862 = ORIENTED_EDGE('',*,*,#4935,.F.) ;
#6863 = ORIENTED_EDGE('',*,*,#4937,.F.) ;
#6864 = ORIENTED_EDGE('',*,*,#4931,.F.) ;
#6865 = ORIENTED_EDGE('',*,*,#4940,.T.) ;
#6866 = ORIENTED_EDGE('',*,*,#4936,.F.) ;
#6867 = ORIENTED_EDGE('',*,*,#4939,.F.) ;
#6868 = ORIENTED_EDGE('',*,*,#4930,.F.) ;
#6869 = ORIENTED_EDGE('',*,*,#4938,.T.) ;
#6870 = ORIENTED_EDGE('',*,*,#4933,.F.) ;
#6871 = ORIENTED_EDGE('',*,*,#4940,.F.) ;
#6872 = ORIENTED_EDGE('',*,*,#4929,.F.) ;
#6873 = ORIENTED_EDGE('',*,*,#4941,.F.) ;
#6874 = ORIENTED_EDGE('',*,*,#4942,.T.) ;
#6875 = ORIENTED_EDGE('',*,*,#4943,.F.) ;
#6876 = ORIENTED_EDGE('',*,*,#4942,.F.) ;
#6877 = ORIENTED_EDGE('',*,*,#4943,.T.) ;
#6878 = ORIENTED_EDGE('',*,*,#4941,.T.) ;
#6879 = ORIENTED_EDGE('',*,*,#4944,.F.) ;
#6880 = ORIENTED_EDGE('',*,*,#4945,.T.) ;
#6881 = ORIENTED_EDGE('',*,*,#4946,.F.) ;
#6882 = ORIENTED_EDGE('',*,*,#4945,.F.) ;
#6883 = ORIENTED_EDGE('',*,*,#4946,.T.) ;
#6884 = ORIENTED_EDGE('',*,*,#4944,.T.) ;
#6885 = ORIENTED_EDGE('',*,*,#4947,.F.) ;
#6886 = ORIENTED_EDGE('',*,*,#4948,.T.) ;
#6887 = ORIENTED_EDGE('',*,*,#4949,.F.) ;
#6888 = ORIENTED_EDGE('',*,*,#4948,.F.) ;
#6889 = ORIENTED_EDGE('',*,*,#4949,.T.) ;
#6890 = ORIENTED_EDGE('',*,*,#4947,.T.) ;
#6891 = ORIENTED_EDGE('',*,*,#4950,.F.) ;
#6892 = ORIENTED_EDGE('',*,*,#4951,.T.) ;
#6893 = ORIENTED_EDGE('',*,*,#4952,.F.) ;
#6894 = ORIENTED_EDGE('',*,*,#4951,.F.) ;
#6895 = ORIENTED_EDGE('',*,*,#4952,.T.) ;
#6896 = ORIENTED_EDGE('',*,*,#4950,.T.) ;
#6897 = ORIENTED_EDGE('',*,*,#4953,.T.) ;
#6898 = ORIENTED_EDGE('',*,*,#4954,.T.) ;
#6899 = ORIENTED_EDGE('',*,*,#4955,.T.) ;
#6900 = ORIENTED_EDGE('',*,*,#4956,.T.) ;
#6901 = ORIENTED_EDGE('',*,*,#4957,.T.) ;
#6902 = ORIENTED_EDGE('',*,*,#4958,.T.) ;
#6903 = ORIENTED_EDGE('',*,*,#4959,.T.) ;
#6904 = ORIENTED_EDGE('',*,*,#4960,.T.) ;
#6905 = ORIENTED_EDGE('',*,*,#4961,.T.) ;
#6906 = ORIENTED_EDGE('',*,*,#4962,.T.) ;
#6907 = ORIENTED_EDGE('',*,*,#4963,.T.) ;
#6908 = ORIENTED_EDGE('',*,*,#4964,.T.) ;
#6909 = ORIENTED_EDGE('',*,*,#4965,.T.) ;
#6910 = ORIENTED_EDGE('',*,*,#4966,.T.) ;
#6911 = ORIENTED_EDGE('',*,*,#4967,.T.) ;
#6912 = ORIENTED_EDGE('',*,*,#4968,.T.) ;
#6913 = ORIENTED_EDGE('',*,*,#4969,.T.) ;
#6914 = ORIENTED_EDGE('',*,*,#4970,.T.) ;
#6915 = ORIENTED_EDGE('',*,*,#4971,.T.) ;
#6916 = ORIENTED_EDGE('',*,*,#4972,.T.) ;
#6917 = ORIENTED_EDGE('',*,*,#4973,.T.) ;
#6918 = ORIENTED_EDGE('',*,*,#4974,.T.) ;
#6919 = ORIENTED_EDGE('',*,*,#4975,.T.) ;
#6920 = ORIENTED_EDGE('',*,*,#4976,.T.) ;
#6921 = ORIENTED_EDGE('',*,*,#4977,.T.) ;
#6922 = ORIENTED_EDGE('',*,*,#4978,.T.) ;
#6923 = ORIENTED_EDGE('',*,*,#4979,.T.) ;
#6924 = ORIENTED_EDGE('',*,*,#4980,.T.) ;
#6925 = ORIENTED_EDGE('',*,*,#4981,.T.) ;
#6926 = ORIENTED_EDGE('',*,*,#4982,.T.) ;
#6927 = ORIENTED_EDGE('',*,*,#4983,.T.) ;
#6928 = ORIENTED_EDGE('',*,*,#4984,.T.) ;
#6929 = ORIENTED_EDGE('',*,*,#4985,.T.) ;
#6930 = ORIENTED_EDGE('',*,*,#4986,.T.) ;
#6931 = ORIENTED_EDGE('',*,*,#4987,.T.) ;
#6932 = ORIENTED_EDGE('',*,*,#4988,.T.) ;
#6933 = ORIENTED_EDGE('',*,*,#4989,.T.) ;
#6934 = ORIENTED_EDGE('',*,*,#4990,.T.) ;
#6935 = ORIENTED_EDGE('',*,*,#4991,.T.) ;
#6936 = ORIENTED_EDGE('',*,*,#4992,.T.) ;
#6937 = ORIENTED_EDGE('',*,*,#4993,.T.) ;
#6938 = ORIENTED_EDGE('',*,*,#4994,.T.) ;
#6939 = ORIENTED_EDGE('',*,*,#4995,.T.) ;
#6940 = ORIENTED_EDGE('',*,*,#4996,.T.) ;
#6941 = ORIENTED_EDGE('',*,*,#4997,.T.) ;
#6942 = ORIENTED_EDGE('',*,*,#4998,.T.) ;
#6943 = ORIENTED_EDGE('',*,*,#4999,.T.) ;
#6944 = ORIENTED_EDGE('',*,*,#5000,.T.) ;
#6945 = ORIENTED_EDGE('',*,*,#5001,.T.) ;
#6946 = ORIENTED_EDGE('',*,*,#5002,.T.) ;
#6947 = ORIENTED_EDGE('',*,*,#5003,.T.) ;
#6948 = ORIENTED_EDGE('',*,*,#5004,.T.) ;
#6949 = ORIENTED_EDGE('',*,*,#5005,.T.) ;
#6950 = ORIENTED_EDGE('',*,*,#5006,.T.) ;
#6951 = ORIENTED_EDGE('',*,*,#5007,.T.) ;
#6952 = ORIENTED_EDGE('',*,*,#5008,.T.) ;
#6953 = ORIENTED_EDGE('',*,*,#5009,.T.) ;
#6954 = ORIENTED_EDGE('',*,*,#5010,.T.) ;
#6955 = ORIENTED_EDGE('',*,*,#5011,.T.) ;
#6956 = ORIENTED_EDGE('',*,*,#5012,.T.) ;
#6957 = ORIENTED_EDGE('',*,*,#5013,.T.) ;
#6958 = ORIENTED_EDGE('',*,*,#5014,.T.) ;
#6959 = ORIENTED_EDGE('',*,*,#5015,.T.) ;
#6960 = ORIENTED_EDGE('',*,*,#5016,.T.) ;
#6961 = ORIENTED_EDGE('',*,*,#5017,.T.) ;
#6962 = ORIENTED_EDGE('',*,*,#5018,.T.) ;
#6963 = ORIENTED_EDGE('',*,*,#5019,.T.) ;
#6964 = ORIENTED_EDGE('',*,*,#5020,.T.) ;
#6965 = ORIENTED_EDGE('',*,*,#5021,.T.) ;
#6966 = ORIENTED_EDGE('',*,*,#5022,.T.) ;
#6967 = ORIENTED_EDGE('',*,*,#5023,.T.) ;
#6968 = ORIENTED_EDGE('',*,*,#5024,.T.) ;
#6969 = ORIENTED_EDGE('',*,*,#5025,.T.) ;
#6970 = ORIENTED_EDGE('',*,*,#5026,.T.) ;
#6971 = ORIENTED_EDGE('',*,*,#5027,.T.) ;
#6972 = ORIENTED_EDGE('',*,*,#5028,.T.) ;
#6973 = ORIENTED_EDGE('',*,*,#5029,.T.) ;
#6974 = ORIENTED_EDGE('',*,*,#5030,.T.) ;
#6975 = ORIENTED_EDGE('',*,*,#5031,.T.) ;
#6976 = ORIENTED_EDGE('',*,*,#5032,.T.) ;
#6977 = ORIENTED_EDGE('',*,*,#5033,.T.) ;
#6978 = ORIENTED_EDGE('',*,*,#5034,.T.) ;
#6979 = ORIENTED_EDGE('',*,*,#5035,.T.) ;
#6980 = ORIENTED_EDGE('',*,*,#5036,.T.) ;
#6981 = ORIENTED_EDGE('',*,*,#5037,.T.) ;
#6982 = ORIENTED_EDGE('',*,*,#5038,.T.) ;
#6983 = ORIENTED_EDGE('',*,*,#5039,.T.) ;
#6984 = ORIENTED_EDGE('',*,*,#5040,.T.) ;
#6985 = ORIENTED_EDGE('',*,*,#5041,.T.) ;
#6986 = ORIENTED_EDGE('',*,*,#5042,.T.) ;
#6987 = ORIENTED_EDGE('',*,*,#5043,.T.) ;
#6988 = ORIENTED_EDGE('',*,*,#5044,.T.) ;
#6989 = ORIENTED_EDGE('',*,*,#5045,.T.) ;
#6990 = ORIENTED_EDGE('',*,*,#5046,.T.) ;
#6991 = ORIENTED_EDGE('',*,*,#5047,.F.) ;
#6992 = ORIENTED_EDGE('',*,*,#5048,.T.) ;
#6993 = ORIENTED_EDGE('',*,*,#5049,.F.) ;
#6994 = ORIENTED_EDGE('',*,*,#5050,.F.) ;
#6995 = ORIENTED_EDGE('',*,*,#4953,.F.) ;
#6996 = ORIENTED_EDGE('',*,*,#5051,.F.) ;
#6997 = ORIENTED_EDGE('',*,*,#5048,.F.) ;
#6998 = ORIENTED_EDGE('',*,*,#5047,.T.) ;
#6999 = ORIENTED_EDGE('',*,*,#5050,.T.) ;
#7000 = ORIENTED_EDGE('',*,*,#5052,.T.) ;
#7001 = ORIENTED_EDGE('',*,*,#5053,.F.) ;
#7002 = ORIENTED_EDGE('',*,*,#4955,.F.) ;
#7003 = ORIENTED_EDGE('',*,*,#5054,.F.) ;
#7004 = ORIENTED_EDGE('',*,*,#5052,.F.) ;
#7005 = ORIENTED_EDGE('',*,*,#5049,.T.) ;
#7006 = ORIENTED_EDGE('',*,*,#5051,.T.) ;
#7007 = ORIENTED_EDGE('',*,*,#4954,.F.) ;
#7008 = ORIENTED_EDGE('',*,*,#5053,.T.) ;
#7009 = ORIENTED_EDGE('',*,*,#5054,.T.) ;
#7010 = ORIENTED_EDGE('',*,*,#4957,.F.) ;
#7011 = ORIENTED_EDGE('',*,*,#5055,.T.) ;
#7012 = ORIENTED_EDGE('',*,*,#4958,.F.) ;
#7013 = ORIENTED_EDGE('',*,*,#5056,.F.) ;
#7014 = ORIENTED_EDGE('',*,*,#4959,.F.) ;
#7015 = ORIENTED_EDGE('',*,*,#5055,.F.) ;
#7016 = ORIENTED_EDGE('',*,*,#4956,.F.) ;
#7017 = ORIENTED_EDGE('',*,*,#5056,.T.) ;
#7018 = ORIENTED_EDGE('',*,*,#4961,.F.) ;
#7019 = ORIENTED_EDGE('',*,*,#5057,.T.) ;
#7020 = ORIENTED_EDGE('',*,*,#4962,.F.) ;
#7021 = ORIENTED_EDGE('',*,*,#5058,.F.) ;
#7022 = ORIENTED_EDGE('',*,*,#4963,.F.) ;
#7023 = ORIENTED_EDGE('',*,*,#5057,.F.) ;
#7024 = ORIENTED_EDGE('',*,*,#4960,.F.) ;
#7025 = ORIENTED_EDGE('',*,*,#5058,.T.) ;
#7026 = ORIENTED_EDGE('',*,*,#4965,.F.) ;
#7027 = ORIENTED_EDGE('',*,*,#5059,.T.) ;
#7028 = ORIENTED_EDGE('',*,*,#4966,.F.) ;
#7029 = ORIENTED_EDGE('',*,*,#5060,.F.) ;
#7030 = ORIENTED_EDGE('',*,*,#4967,.F.) ;
#7031 = ORIENTED_EDGE('',*,*,#5059,.F.) ;
#7032 = ORIENTED_EDGE('',*,*,#4964,.F.) ;
#7033 = ORIENTED_EDGE('',*,*,#5060,.T.) ;
#7034 = ORIENTED_EDGE('',*,*,#4969,.F.) ;
#7035 = ORIENTED_EDGE('',*,*,#5061,.T.) ;
#7036 = ORIENTED_EDGE('',*,*,#4970,.F.) ;
#7037 = ORIENTED_EDGE('',*,*,#5062,.F.) ;
#7038 = ORIENTED_EDGE('',*,*,#5063,.F.) ;
#7039 = ORIENTED_EDGE('',*,*,#4971,.F.) ;
#7040 = ORIENTED_EDGE('',*,*,#5061,.F.) ;
#7041 = ORIENTED_EDGE('',*,*,#4968,.F.) ;
#7042 = ORIENTED_EDGE('',*,*,#5063,.T.) ;
#7043 = ORIENTED_EDGE('',*,*,#5064,.T.) ;
#7044 = ORIENTED_EDGE('',*,*,#5065,.F.) ;
#7045 = ORIENTED_EDGE('',*,*,#5066,.F.) ;
#7046 = ORIENTED_EDGE('',*,*,#4973,.F.) ;
#7047 = ORIENTED_EDGE('',*,*,#5067,.F.) ;
#7048 = ORIENTED_EDGE('',*,*,#5064,.F.) ;
#7049 = ORIENTED_EDGE('',*,*,#5062,.T.) ;
#7050 = ORIENTED_EDGE('',*,*,#4972,.F.) ;
#7051 = ORIENTED_EDGE('',*,*,#5066,.T.) ;
#7052 = ORIENTED_EDGE('',*,*,#5068,.T.) ;
#7053 = ORIENTED_EDGE('',*,*,#5069,.F.) ;
#7054 = ORIENTED_EDGE('',*,*,#4975,.F.) ;
#7055 = ORIENTED_EDGE('',*,*,#5070,.F.) ;
#7056 = ORIENTED_EDGE('',*,*,#5068,.F.) ;
#7057 = ORIENTED_EDGE('',*,*,#5065,.T.) ;
#7058 = ORIENTED_EDGE('',*,*,#5067,.T.) ;
#7059 = ORIENTED_EDGE('',*,*,#4974,.F.) ;
#7060 = ORIENTED_EDGE('',*,*,#5069,.T.) ;
#7061 = ORIENTED_EDGE('',*,*,#5071,.T.) ;
#7062 = ORIENTED_EDGE('',*,*,#5072,.F.) ;
#7063 = ORIENTED_EDGE('',*,*,#5073,.F.) ;
#7064 = ORIENTED_EDGE('',*,*,#4977,.F.) ;
#7065 = ORIENTED_EDGE('',*,*,#5074,.F.) ;
#7066 = ORIENTED_EDGE('',*,*,#5071,.F.) ;
#7067 = ORIENTED_EDGE('',*,*,#5070,.T.) ;
#7068 = ORIENTED_EDGE('',*,*,#4976,.F.) ;
#7069 = ORIENTED_EDGE('',*,*,#5073,.T.) ;
#7070 = ORIENTED_EDGE('',*,*,#5075,.T.) ;
#7071 = ORIENTED_EDGE('',*,*,#5076,.F.) ;
#7072 = ORIENTED_EDGE('',*,*,#4979,.F.) ;
#7073 = ORIENTED_EDGE('',*,*,#5077,.F.) ;
#7074 = ORIENTED_EDGE('',*,*,#5075,.F.) ;
#7075 = ORIENTED_EDGE('',*,*,#5072,.T.) ;
#7076 = ORIENTED_EDGE('',*,*,#5074,.T.) ;
#7077 = ORIENTED_EDGE('',*,*,#4978,.F.) ;
#7078 = ORIENTED_EDGE('',*,*,#5076,.T.) ;
#7079 = ORIENTED_EDGE('',*,*,#5077,.T.) ;
#7080 = ORIENTED_EDGE('',*,*,#4981,.F.) ;
#7081 = ORIENTED_EDGE('',*,*,#5078,.T.) ;
#7082 = ORIENTED_EDGE('',*,*,#4982,.F.) ;
#7083 = ORIENTED_EDGE('',*,*,#5079,.F.) ;
#7084 = ORIENTED_EDGE('',*,*,#4983,.F.) ;
#7085 = ORIENTED_EDGE('',*,*,#5078,.F.) ;
#7086 = ORIENTED_EDGE('',*,*,#4980,.F.) ;
#7087 = ORIENTED_EDGE('',*,*,#5079,.T.) ;
#7088 = ORIENTED_EDGE('',*,*,#4985,.F.) ;
#7089 = ORIENTED_EDGE('',*,*,#5080,.T.) ;
#7090 = ORIENTED_EDGE('',*,*,#4986,.F.) ;
#7091 = ORIENTED_EDGE('',*,*,#5081,.F.) ;
#7092 = ORIENTED_EDGE('',*,*,#4987,.F.) ;
#7093 = ORIENTED_EDGE('',*,*,#5080,.F.) ;
#7094 = ORIENTED_EDGE('',*,*,#4984,.F.) ;
#7095 = ORIENTED_EDGE('',*,*,#5081,.T.) ;
#7096 = ORIENTED_EDGE('',*,*,#4989,.F.) ;
#7097 = ORIENTED_EDGE('',*,*,#5082,.T.) ;
#7098 = ORIENTED_EDGE('',*,*,#4990,.F.) ;
#7099 = ORIENTED_EDGE('',*,*,#5083,.F.) ;
#7100 = ORIENTED_EDGE('',*,*,#4991,.F.) ;
#7101 = ORIENTED_EDGE('',*,*,#5082,.F.) ;
#7102 = ORIENTED_EDGE('',*,*,#4988,.F.) ;
#7103 = ORIENTED_EDGE('',*,*,#5083,.T.) ;
#7104 = ORIENTED_EDGE('',*,*,#4993,.F.) ;
#7105 = ORIENTED_EDGE('',*,*,#5084,.T.) ;
#7106 = ORIENTED_EDGE('',*,*,#4994,.F.) ;
#7107 = ORIENTED_EDGE('',*,*,#5085,.F.) ;
#7108 = ORIENTED_EDGE('',*,*,#5086,.F.) ;
#7109 = ORIENTED_EDGE('',*,*,#4995,.F.) ;
#7110 = ORIENTED_EDGE('',*,*,#5084,.F.) ;
#7111 = ORIENTED_EDGE('',*,*,#4992,.F.) ;
#7112 = ORIENTED_EDGE('',*,*,#5086,.T.) ;
#7113 = ORIENTED_EDGE('',*,*,#5087,.T.) ;
#7114 = ORIENTED_EDGE('',*,*,#5088,.F.) ;
#7115 = ORIENTED_EDGE('',*,*,#5089,.F.) ;
#7116 = ORIENTED_EDGE('',*,*,#4997,.F.) ;
#7117 = ORIENTED_EDGE('',*,*,#5090,.F.) ;
#7118 = ORIENTED_EDGE('',*,*,#5087,.F.) ;
#7119 = ORIENTED_EDGE('',*,*,#5085,.T.) ;
#7120 = ORIENTED_EDGE('',*,*,#4996,.F.) ;
#7121 = ORIENTED_EDGE('',*,*,#5089,.T.) ;
#7122 = ORIENTED_EDGE('',*,*,#5091,.T.) ;
#7123 = ORIENTED_EDGE('',*,*,#5092,.F.) ;
#7124 = ORIENTED_EDGE('',*,*,#4999,.F.) ;
#7125 = ORIENTED_EDGE('',*,*,#5093,.F.) ;
#7126 = ORIENTED_EDGE('',*,*,#5091,.F.) ;
#7127 = ORIENTED_EDGE('',*,*,#5088,.T.) ;
#7128 = ORIENTED_EDGE('',*,*,#5090,.T.) ;
#7129 = ORIENTED_EDGE('',*,*,#4998,.F.) ;
#7130 = ORIENTED_EDGE('',*,*,#5092,.T.) ;
#7131 = ORIENTED_EDGE('',*,*,#5094,.T.) ;
#7132 = ORIENTED_EDGE('',*,*,#5095,.F.) ;
#7133 = ORIENTED_EDGE('',*,*,#5096,.F.) ;
#7134 = ORIENTED_EDGE('',*,*,#5001,.F.) ;
#7135 = ORIENTED_EDGE('',*,*,#5097,.F.) ;
#7136 = ORIENTED_EDGE('',*,*,#5094,.F.) ;
#7137 = ORIENTED_EDGE('',*,*,#5093,.T.) ;
#7138 = ORIENTED_EDGE('',*,*,#5000,.F.) ;
#7139 = ORIENTED_EDGE('',*,*,#5096,.T.) ;
#7140 = ORIENTED_EDGE('',*,*,#5098,.T.) ;
#7141 = ORIENTED_EDGE('',*,*,#5099,.F.) ;
#7142 = ORIENTED_EDGE('',*,*,#5003,.F.) ;
#7143 = ORIENTED_EDGE('',*,*,#5100,.F.) ;
#7144 = ORIENTED_EDGE('',*,*,#5098,.F.) ;
#7145 = ORIENTED_EDGE('',*,*,#5095,.T.) ;
#7146 = ORIENTED_EDGE('',*,*,#5097,.T.) ;
#7147 = ORIENTED_EDGE('',*,*,#5002,.F.) ;
#7148 = ORIENTED_EDGE('',*,*,#5099,.T.) ;
#7149 = ORIENTED_EDGE('',*,*,#5100,.T.) ;
#7150 = ORIENTED_EDGE('',*,*,#5005,.F.) ;
#7151 = ORIENTED_EDGE('',*,*,#5101,.T.) ;
#7152 = ORIENTED_EDGE('',*,*,#5006,.F.) ;
#7153 = ORIENTED_EDGE('',*,*,#5102,.F.) ;
#7154 = ORIENTED_EDGE('',*,*,#5007,.F.) ;
#7155 = ORIENTED_EDGE('',*,*,#5101,.F.) ;
#7156 = ORIENTED_EDGE('',*,*,#5004,.F.) ;
#7157 = ORIENTED_EDGE('',*,*,#5102,.T.) ;
#7158 = ORIENTED_EDGE('',*,*,#5009,.F.) ;
#7159 = ORIENTED_EDGE('',*,*,#5103,.T.) ;
#7160 = ORIENTED_EDGE('',*,*,#5010,.F.) ;
#7161 = ORIENTED_EDGE('',*,*,#5104,.F.) ;
#7162 = ORIENTED_EDGE('',*,*,#5011,.F.) ;
#7163 = ORIENTED_EDGE('',*,*,#5103,.F.) ;
#7164 = ORIENTED_EDGE('',*,*,#5008,.F.) ;
#7165 = ORIENTED_EDGE('',*,*,#5104,.T.) ;
#7166 = ORIENTED_EDGE('',*,*,#5013,.F.) ;
#7167 = ORIENTED_EDGE('',*,*,#5105,.T.) ;
#7168 = ORIENTED_EDGE('',*,*,#5014,.F.) ;
#7169 = ORIENTED_EDGE('',*,*,#5106,.F.) ;
#7170 = ORIENTED_EDGE('',*,*,#5015,.F.) ;
#7171 = ORIENTED_EDGE('',*,*,#5105,.F.) ;
#7172 = ORIENTED_EDGE('',*,*,#5012,.F.) ;
#7173 = ORIENTED_EDGE('',*,*,#5106,.T.) ;
#7174 = ORIENTED_EDGE('',*,*,#5017,.F.) ;
#7175 = ORIENTED_EDGE('',*,*,#5107,.T.) ;
#7176 = ORIENTED_EDGE('',*,*,#5018,.F.) ;
#7177 = ORIENTED_EDGE('',*,*,#5108,.F.) ;
#7178 = ORIENTED_EDGE('',*,*,#5109,.F.) ;
#7179 = ORIENTED_EDGE('',*,*,#5019,.F.) ;
#7180 = ORIENTED_EDGE('',*,*,#5107,.F.) ;
#7181 = ORIENTED_EDGE('',*,*,#5016,.F.) ;
#7182 = ORIENTED_EDGE('',*,*,#5109,.T.) ;
#7183 = ORIENTED_EDGE('',*,*,#5110,.T.) ;
#7184 = ORIENTED_EDGE('',*,*,#5111,.F.) ;
#7185 = ORIENTED_EDGE('',*,*,#5112,.F.) ;
#7186 = ORIENTED_EDGE('',*,*,#5021,.F.) ;
#7187 = ORIENTED_EDGE('',*,*,#5113,.F.) ;
#7188 = ORIENTED_EDGE('',*,*,#5110,.F.) ;
#7189 = ORIENTED_EDGE('',*,*,#5108,.T.) ;
#7190 = ORIENTED_EDGE('',*,*,#5020,.F.) ;
#7191 = ORIENTED_EDGE('',*,*,#5112,.T.) ;
#7192 = ORIENTED_EDGE('',*,*,#5114,.T.) ;
#7193 = ORIENTED_EDGE('',*,*,#5115,.F.) ;
#7194 = ORIENTED_EDGE('',*,*,#5023,.F.) ;
#7195 = ORIENTED_EDGE('',*,*,#5116,.F.) ;
#7196 = ORIENTED_EDGE('',*,*,#5114,.F.) ;
#7197 = ORIENTED_EDGE('',*,*,#5111,.T.) ;
#7198 = ORIENTED_EDGE('',*,*,#5113,.T.) ;
#7199 = ORIENTED_EDGE('',*,*,#5022,.F.) ;
#7200 = ORIENTED_EDGE('',*,*,#5115,.T.) ;
#7201 = ORIENTED_EDGE('',*,*,#5117,.T.) ;
#7202 = ORIENTED_EDGE('',*,*,#5118,.F.) ;
#7203 = ORIENTED_EDGE('',*,*,#5119,.F.) ;
#7204 = ORIENTED_EDGE('',*,*,#5025,.F.) ;
#7205 = ORIENTED_EDGE('',*,*,#5120,.F.) ;
#7206 = ORIENTED_EDGE('',*,*,#5117,.F.) ;
#7207 = ORIENTED_EDGE('',*,*,#5116,.T.) ;
#7208 = ORIENTED_EDGE('',*,*,#5024,.F.) ;
#7209 = ORIENTED_EDGE('',*,*,#5119,.T.) ;
#7210 = ORIENTED_EDGE('',*,*,#5121,.T.) ;
#7211 = ORIENTED_EDGE('',*,*,#5122,.F.) ;
#7212 = ORIENTED_EDGE('',*,*,#5027,.F.) ;
#7213 = ORIENTED_EDGE('',*,*,#5123,.F.) ;
#7214 = ORIENTED_EDGE('',*,*,#5121,.F.) ;
#7215 = ORIENTED_EDGE('',*,*,#5118,.T.) ;
#7216 = ORIENTED_EDGE('',*,*,#5120,.T.) ;
#7217 = ORIENTED_EDGE('',*,*,#5026,.F.) ;
#7218 = ORIENTED_EDGE('',*,*,#5122,.T.) ;
#7219 = ORIENTED_EDGE('',*,*,#5123,.T.) ;
#7220 = ORIENTED_EDGE('',*,*,#5029,.F.) ;
#7221 = ORIENTED_EDGE('',*,*,#5124,.T.) ;
#7222 = ORIENTED_EDGE('',*,*,#5030,.F.) ;
#7223 = ORIENTED_EDGE('',*,*,#5125,.F.) ;
#7224 = ORIENTED_EDGE('',*,*,#5031,.F.) ;
#7225 = ORIENTED_EDGE('',*,*,#5124,.F.) ;
#7226 = ORIENTED_EDGE('',*,*,#5028,.F.) ;
#7227 = ORIENTED_EDGE('',*,*,#5125,.T.) ;
#7228 = ORIENTED_EDGE('',*,*,#5033,.F.) ;
#7229 = ORIENTED_EDGE('',*,*,#5126,.T.) ;
#7230 = ORIENTED_EDGE('',*,*,#5034,.F.) ;
#7231 = ORIENTED_EDGE('',*,*,#5127,.F.) ;
#7232 = ORIENTED_EDGE('',*,*,#5035,.F.) ;
#7233 = ORIENTED_EDGE('',*,*,#5126,.F.) ;
#7234 = ORIENTED_EDGE('',*,*,#5032,.F.) ;
#7235 = ORIENTED_EDGE('',*,*,#5127,.T.) ;
#7236 = ORIENTED_EDGE('',*,*,#5037,.F.) ;
#7237 = ORIENTED_EDGE('',*,*,#5128,.T.) ;
#7238 = ORIENTED_EDGE('',*,*,#5038,.F.) ;
#7239 = ORIENTED_EDGE('',*,*,#5129,.F.) ;
#7240 = ORIENTED_EDGE('',*,*,#5039,.F.) ;
#7241 = ORIENTED_EDGE('',*,*,#5128,.F.) ;
#7242 = ORIENTED_EDGE('',*,*,#5036,.F.) ;
#7243 = ORIENTED_EDGE('',*,*,#5129,.T.) ;
#7244 = ORIENTED_EDGE('',*,*,#5041,.F.) ;
#7245 = ORIENTED_EDGE('',*,*,#5130,.T.) ;
#7246 = ORIENTED_EDGE('',*,*,#5042,.F.) ;
#7247 = ORIENTED_EDGE('',*,*,#5131,.F.) ;
#7248 = ORIENTED_EDGE('',*,*,#5132,.F.) ;
#7249 = ORIENTED_EDGE('',*,*,#5043,.F.) ;
#7250 = ORIENTED_EDGE('',*,*,#5130,.F.) ;
#7251 = ORIENTED_EDGE('',*,*,#5040,.F.) ;
#7252 = ORIENTED_EDGE('',*,*,#5132,.T.) ;
#7253 = ORIENTED_EDGE('',*,*,#5133,.T.) ;
#7254 = ORIENTED_EDGE('',*,*,#5134,.F.) ;
#7255 = ORIENTED_EDGE('',*,*,#5135,.F.) ;
#7256 = ORIENTED_EDGE('',*,*,#5045,.F.) ;
#7257 = ORIENTED_EDGE('',*,*,#5136,.F.) ;
#7258 = ORIENTED_EDGE('',*,*,#5133,.F.) ;
#7259 = ORIENTED_EDGE('',*,*,#5131,.T.) ;
#7260 = ORIENTED_EDGE('',*,*,#5044,.F.) ;
#7261 = ORIENTED_EDGE('',*,*,#5135,.T.) ;
#7262 = ORIENTED_EDGE('',*,*,#5137,.T.) ;
#7263 = ORIENTED_EDGE('',*,*,#5138,.F.) ;
#7264 = ORIENTED_EDGE('',*,*,#5137,.F.) ;
#7265 = ORIENTED_EDGE('',*,*,#5134,.T.) ;
#7266 = ORIENTED_EDGE('',*,*,#5136,.T.) ;
#7267 = ORIENTED_EDGE('',*,*,#5046,.F.) ;
#7268 = ORIENTED_EDGE('',*,*,#5138,.T.) ;
#7269 = ORIENTED_EDGE('',*,*,#5139,.F.) ;
#7270 = ORIENTED_EDGE('',*,*,#5140,.T.) ;
#7271 = ORIENTED_EDGE('',*,*,#5141,.F.) ;
#7272 = ORIENTED_EDGE('',*,*,#5140,.F.) ;
#7273 = ORIENTED_EDGE('',*,*,#5142,.F.) ;
#7274 = ORIENTED_EDGE('',*,*,#5143,.F.) ;
#7275 = ORIENTED_EDGE('',*,*,#5144,.F.) ;
#7276 = ORIENTED_EDGE('',*,*,#5145,.T.) ;
#7277 = ORIENTED_EDGE('',*,*,#5139,.T.) ;
#7278 = ORIENTED_EDGE('',*,*,#5146,.T.) ;
#7279 = ORIENTED_EDGE('',*,*,#5147,.T.) ;
#7280 = ORIENTED_EDGE('',*,*,#5144,.T.) ;
#7281 = ORIENTED_EDGE('',*,*,#5148,.T.) ;
#7282 = ORIENTED_EDGE('',*,*,#5149,.F.) ;
#7283 = ORIENTED_EDGE('',*,*,#5150,.F.) ;
#7284 = ORIENTED_EDGE('',*,*,#5146,.F.) ;
#7285 = ORIENTED_EDGE('',*,*,#5151,.T.) ;
#7286 = ORIENTED_EDGE('',*,*,#5141,.T.) ;
#7287 = ORIENTED_EDGE('',*,*,#5152,.T.) ;
#7288 = ORIENTED_EDGE('',*,*,#5153,.T.) ;
#7289 = ORIENTED_EDGE('',*,*,#5154,.T.) ;
#7290 = ORIENTED_EDGE('',*,*,#5155,.T.) ;
#7291 = ORIENTED_EDGE('',*,*,#5149,.T.) ;
#7292 = ORIENTED_EDGE('',*,*,#5156,.T.) ;
#7293 = ORIENTED_EDGE('',*,*,#5157,.T.) ;
#7294 = ORIENTED_EDGE('',*,*,#5158,.T.) ;
#7295 = ORIENTED_EDGE('',*,*,#5142,.T.) ;
#7296 = ORIENTED_EDGE('',*,*,#5159,.T.) ;
#7297 = ORIENTED_EDGE('',*,*,#5160,.T.) ;
#7298 = ORIENTED_EDGE('',*,*,#5161,.T.) ;
#7299 = ORIENTED_EDGE('',*,*,#5154,.F.) ;
#7300 = ORIENTED_EDGE('',*,*,#5162,.F.) ;
#7301 = ORIENTED_EDGE('',*,*,#5156,.F.) ;
#7302 = ORIENTED_EDGE('',*,*,#5151,.F.) ;
#7303 = ORIENTED_EDGE('',*,*,#5148,.F.) ;
#7304 = ORIENTED_EDGE('',*,*,#5143,.T.) ;
#7305 = ORIENTED_EDGE('',*,*,#5161,.F.) ;
#7306 = ORIENTED_EDGE('',*,*,#5163,.T.) ;
#7307 = ORIENTED_EDGE('',*,*,#5164,.T.) ;
#7308 = ORIENTED_EDGE('',*,*,#5155,.F.) ;
#7309 = ORIENTED_EDGE('',*,*,#5163,.F.) ;
#7310 = ORIENTED_EDGE('',*,*,#5160,.F.) ;
#7311 = ORIENTED_EDGE('',*,*,#5152,.F.) ;
#7312 = ORIENTED_EDGE('',*,*,#5164,.F.) ;
#7313 = ORIENTED_EDGE('',*,*,#5159,.F.) ;
#7314 = ORIENTED_EDGE('',*,*,#5145,.F.) ;
#7315 = ORIENTED_EDGE('',*,*,#5147,.F.) ;
#7316 = ORIENTED_EDGE('',*,*,#5150,.T.) ;
#7317 = ORIENTED_EDGE('',*,*,#5158,.F.) ;
#7318 = ORIENTED_EDGE('',*,*,#5165,.T.) ;
#7319 = ORIENTED_EDGE('',*,*,#5162,.T.) ;
#7320 = ORIENTED_EDGE('',*,*,#5153,.F.) ;
#7321 = ORIENTED_EDGE('',*,*,#5165,.F.) ;
#7322 = ORIENTED_EDGE('',*,*,#5157,.F.) ;
#7323 = ORIENTED_EDGE('',*,*,#5166,.F.) ;
#7324 = ORIENTED_EDGE('',*,*,#5167,.F.) ;
#7325 = ORIENTED_EDGE('',*,*,#5168,.F.) ;
#7326 = ORIENTED_EDGE('',*,*,#5169,.F.) ;
#7327 = ORIENTED_EDGE('',*,*,#5170,.F.) ;
#7328 = ORIENTED_EDGE('',*,*,#5169,.T.) ;
#7329 = ORIENTED_EDGE('',*,*,#5171,.T.) ;
#7330 = ORIENTED_EDGE('',*,*,#5172,.T.) ;
#7331 = ORIENTED_EDGE('',*,*,#5173,.F.) ;
#7332 = ORIENTED_EDGE('',*,*,#5172,.F.) ;
#7333 = ORIENTED_EDGE('',*,*,#5174,.F.) ;
#7334 = ORIENTED_EDGE('',*,*,#5175,.F.) ;
#7335 = ORIENTED_EDGE('',*,*,#5176,.F.) ;
#7336 = ORIENTED_EDGE('',*,*,#5175,.T.) ;
#7337 = ORIENTED_EDGE('',*,*,#5177,.F.) ;
#7338 = ORIENTED_EDGE('',*,*,#5167,.T.) ;
#7339 = ORIENTED_EDGE('',*,*,#5171,.F.) ;
#7340 = ORIENTED_EDGE('',*,*,#5168,.T.) ;
#7341 = ORIENTED_EDGE('',*,*,#5177,.T.) ;
#7342 = ORIENTED_EDGE('',*,*,#5174,.T.) ;
#7343 = ORIENTED_EDGE('',*,*,#5178,.F.) ;
#7344 = ORIENTED_EDGE('',*,*,#5178,.T.) ;
#7345 = ORIENTED_EDGE('',*,*,#5179,.T.) ;
#7346 = ORIENTED_EDGE('',*,*,#5180,.F.) ;
#7347 = ORIENTED_EDGE('',*,*,#5179,.F.) ;
#7348 = ORIENTED_EDGE('',*,*,#5181,.T.) ;
#7349 = ORIENTED_EDGE('',*,*,#5182,.T.) ;
#7350 = ORIENTED_EDGE('',*,*,#5183,.T.) ;
#7351 = ORIENTED_EDGE('',*,*,#5184,.T.) ;
#7352 = ORIENTED_EDGE('',*,*,#5185,.T.) ;
#7353 = ORIENTED_EDGE('',*,*,#5186,.T.) ;
#7354 = ORIENTED_EDGE('',*,*,#5187,.T.) ;
#7355 = ORIENTED_EDGE('',*,*,#5188,.T.) ;
#7356 = ORIENTED_EDGE('',*,*,#5189,.T.) ;
#7357 = ORIENTED_EDGE('',*,*,#5186,.F.) ;
#7358 = ORIENTED_EDGE('',*,*,#5190,.F.) ;
#7359 = ORIENTED_EDGE('',*,*,#5184,.F.) ;
#7360 = ORIENTED_EDGE('',*,*,#5191,.T.) ;
#7361 = ORIENTED_EDGE('',*,*,#5187,.F.) ;
#7362 = ORIENTED_EDGE('',*,*,#5189,.F.) ;
#7363 = ORIENTED_EDGE('',*,*,#5183,.F.) ;
#7364 = ORIENTED_EDGE('',*,*,#5173,.T.) ;
#7365 = ORIENTED_EDGE('',*,*,#5176,.T.) ;
#7366 = ORIENTED_EDGE('',*,*,#5166,.T.) ;
#7367 = ORIENTED_EDGE('',*,*,#5170,.T.) ;
#7368 = ORIENTED_EDGE('',*,*,#5192,.T.) ;
#7369 = ORIENTED_EDGE('',*,*,#5188,.F.) ;
#7370 = ORIENTED_EDGE('',*,*,#5191,.F.) ;
#7371 = ORIENTED_EDGE('',*,*,#5182,.F.) ;
#7372 = ORIENTED_EDGE('',*,*,#5190,.T.) ;
#7373 = ORIENTED_EDGE('',*,*,#5185,.F.) ;
#7374 = ORIENTED_EDGE('',*,*,#5192,.F.) ;
#7375 = ORIENTED_EDGE('',*,*,#5181,.F.) ;
#7376 = ORIENTED_EDGE('',*,*,#5180,.T.) ;
#7377 = ORIENTED_EDGE('',*,*,#5193,.F.) ;
#7378 = ORIENTED_EDGE('',*,*,#5194,.T.) ;
#7379 = ORIENTED_EDGE('',*,*,#5193,.T.) ;
#7380 = ORIENTED_EDGE('',*,*,#5195,.T.) ;
#7381 = ORIENTED_EDGE('',*,*,#5196,.F.) ;
#7382 = ORIENTED_EDGE('',*,*,#5197,.T.) ;
#7383 = ORIENTED_EDGE('',*,*,#5195,.F.) ;
#7384 = ORIENTED_EDGE('',*,*,#5194,.F.) ;
#7385 = ORIENTED_EDGE('',*,*,#5197,.F.) ;
#7386 = ORIENTED_EDGE('',*,*,#5196,.T.) ;
#7387 = ORIENTED_EDGE('',*,*,#5198,.F.) ;
#7388 = ORIENTED_EDGE('',*,*,#5199,.T.) ;
#7389 = ORIENTED_EDGE('',*,*,#5200,.F.) ;
#7390 = ORIENTED_EDGE('',*,*,#5199,.F.) ;
#7391 = ORIENTED_EDGE('',*,*,#5200,.T.) ;
#7392 = ORIENTED_EDGE('',*,*,#5198,.T.) ;
#7393 = ORIENTED_EDGE('',*,*,#5201,.F.) ;
#7394 = ORIENTED_EDGE('',*,*,#5202,.T.) ;
#7395 = ORIENTED_EDGE('',*,*,#5203,.F.) ;
#7396 = ORIENTED_EDGE('',*,*,#5202,.F.) ;
#7397 = ORIENTED_EDGE('',*,*,#5203,.T.) ;
#7398 = ORIENTED_EDGE('',*,*,#5201,.T.) ;
#7399 = ORIENTED_EDGE('',*,*,#5204,.F.) ;
#7400 = ORIENTED_EDGE('',*,*,#5205,.T.) ;
#7401 = ORIENTED_EDGE('',*,*,#5206,.F.) ;
#7402 = ORIENTED_EDGE('',*,*,#5205,.F.) ;
#7403 = ORIENTED_EDGE('',*,*,#5206,.T.) ;
#7404 = ORIENTED_EDGE('',*,*,#5204,.T.) ;
#7405 = ORIENTED_EDGE('',*,*,#5207,.F.) ;
#7406 = ORIENTED_EDGE('',*,*,#5208,.T.) ;
#7407 = ORIENTED_EDGE('',*,*,#5209,.F.) ;
#7408 = ORIENTED_EDGE('',*,*,#5208,.F.) ;
#7409 = ORIENTED_EDGE('',*,*,#5209,.T.) ;
#7410 = ORIENTED_EDGE('',*,*,#5207,.T.) ;
#7411 = ORIENTED_EDGE('',*,*,#5210,.F.) ;
#7412 = ORIENTED_EDGE('',*,*,#5211,.T.) ;
#7413 = ORIENTED_EDGE('',*,*,#5212,.F.) ;
#7414 = ORIENTED_EDGE('',*,*,#5211,.F.) ;
#7415 = ORIENTED_EDGE('',*,*,#5212,.T.) ;
#7416 = ORIENTED_EDGE('',*,*,#5210,.T.) ;
#7417 = ORIENTED_EDGE('',*,*,#5213,.F.) ;
#7418 = ORIENTED_EDGE('',*,*,#5214,.T.) ;
#7419 = ORIENTED_EDGE('',*,*,#5215,.F.) ;
#7420 = ORIENTED_EDGE('',*,*,#5216,.F.) ;
#7421 = ORIENTED_EDGE('',*,*,#5217,.F.) ;
#7422 = ORIENTED_EDGE('',*,*,#5218,.T.) ;
#7423 = ORIENTED_EDGE('',*,*,#5219,.F.) ;
#7424 = ORIENTED_EDGE('',*,*,#5220,.F.) ;
#7425 = ORIENTED_EDGE('',*,*,#5218,.F.) ;
#7426 = ORIENTED_EDGE('',*,*,#5221,.F.) ;
#7427 = ORIENTED_EDGE('',*,*,#5222,.F.) ;
#7428 = ORIENTED_EDGE('',*,*,#5223,.F.) ;
#7429 = ORIENTED_EDGE('',*,*,#5224,.F.) ;
#7430 = ORIENTED_EDGE('',*,*,#5225,.F.) ;
#7431 = ORIENTED_EDGE('',*,*,#5214,.F.) ;
#7432 = ORIENTED_EDGE('',*,*,#5226,.F.) ;
#7433 = ORIENTED_EDGE('',*,*,#5222,.T.) ;
#7434 = ORIENTED_EDGE('',*,*,#5227,.F.) ;
#7435 = ORIENTED_EDGE('',*,*,#5228,.F.) ;
#7436 = ORIENTED_EDGE('',*,*,#5229,.F.) ;
#7437 = ORIENTED_EDGE('',*,*,#5224,.T.) ;
#7438 = ORIENTED_EDGE('',*,*,#5230,.F.) ;
#7439 = ORIENTED_EDGE('',*,*,#5215,.T.) ;
#7440 = ORIENTED_EDGE('',*,*,#5225,.T.) ;
#7441 = ORIENTED_EDGE('',*,*,#5229,.T.) ;
#7442 = ORIENTED_EDGE('',*,*,#5231,.F.) ;
#7443 = ORIENTED_EDGE('',*,*,#5232,.T.) ;
#7444 = ORIENTED_EDGE('',*,*,#5233,.F.) ;
#7445 = ORIENTED_EDGE('',*,*,#5234,.F.) ;
#7446 = ORIENTED_EDGE('',*,*,#5235,.F.) ;
#7447 = ORIENTED_EDGE('',*,*,#5228,.T.) ;
#7448 = ORIENTED_EDGE('',*,*,#5236,.T.) ;
#7449 = ORIENTED_EDGE('',*,*,#5237,.T.) ;
#7450 = ORIENTED_EDGE('',*,*,#5231,.T.) ;
#7451 = ORIENTED_EDGE('',*,*,#5216,.T.) ;
#7452 = ORIENTED_EDGE('',*,*,#5235,.T.) ;
#7453 = ORIENTED_EDGE('',*,*,#5238,.T.) ;
#7454 = ORIENTED_EDGE('',*,*,#5239,.T.) ;
#7455 = ORIENTED_EDGE('',*,*,#5240,.F.) ;
#7456 = ORIENTED_EDGE('',*,*,#5241,.T.) ;
#7457 = ORIENTED_EDGE('',*,*,#5219,.T.) ;
#7458 = ORIENTED_EDGE('',*,*,#5220,.T.) ;
#7459 = ORIENTED_EDGE('',*,*,#5226,.T.) ;
#7460 = ORIENTED_EDGE('',*,*,#5242,.T.) ;
#7461 = ORIENTED_EDGE('',*,*,#5243,.F.) ;
#7462 = ORIENTED_EDGE('',*,*,#5242,.F.) ;
#7463 = ORIENTED_EDGE('',*,*,#5230,.T.) ;
#7464 = ORIENTED_EDGE('',*,*,#5223,.T.) ;
#7465 = ORIENTED_EDGE('',*,*,#5213,.T.) ;
#7466 = ORIENTED_EDGE('',*,*,#5241,.F.) ;
#7467 = ORIENTED_EDGE('',*,*,#5244,.T.) ;
#7468 = ORIENTED_EDGE('',*,*,#5245,.T.) ;
#7469 = ORIENTED_EDGE('',*,*,#5246,.T.) ;
#7470 = ORIENTED_EDGE('',*,*,#5233,.T.) ;
#7471 = ORIENTED_EDGE('',*,*,#5217,.T.) ;
#7472 = ORIENTED_EDGE('',*,*,#5239,.F.) ;
#7473 = ORIENTED_EDGE('',*,*,#5247,.T.) ;
#7474 = ORIENTED_EDGE('',*,*,#5245,.F.) ;
#7475 = ORIENTED_EDGE('',*,*,#5248,.F.) ;
#7476 = ORIENTED_EDGE('',*,*,#5236,.F.) ;
#7477 = ORIENTED_EDGE('',*,*,#5227,.T.) ;
#7478 = ORIENTED_EDGE('',*,*,#5221,.T.) ;
#7479 = ORIENTED_EDGE('',*,*,#5234,.T.) ;
#7480 = ORIENTED_EDGE('',*,*,#5246,.F.) ;
#7481 = ORIENTED_EDGE('',*,*,#5247,.F.) ;
#7482 = ORIENTED_EDGE('',*,*,#5238,.F.) ;
#7483 = ORIENTED_EDGE('',*,*,#5240,.T.) ;
#7484 = ORIENTED_EDGE('',*,*,#5248,.T.) ;
#7485 = ORIENTED_EDGE('',*,*,#5244,.F.) ;
#7486 = ORIENTED_EDGE('',*,*,#5232,.F.) ;
#7487 = ORIENTED_EDGE('',*,*,#5237,.F.) ;
#7488 = ORIENTED_EDGE('',*,*,#5243,.T.) ;
#7489 = ORIENTED_EDGE('',*,*,#5249,.F.) ;
#7490 = ORIENTED_EDGE('',*,*,#5250,.T.) ;
#7491 = ORIENTED_EDGE('',*,*,#5251,.F.) ;
#7492 = ORIENTED_EDGE('',*,*,#5250,.F.) ;
#7493 = ORIENTED_EDGE('',*,*,#5251,.T.) ;
#7494 = ORIENTED_EDGE('',*,*,#5249,.T.) ;
#7495 = ORIENTED_EDGE('',*,*,#5252,.F.) ;
#7496 = ORIENTED_EDGE('',*,*,#5253,.T.) ;
#7497 = ORIENTED_EDGE('',*,*,#5254,.F.) ;
#7498 = ORIENTED_EDGE('',*,*,#5253,.F.) ;
#7499 = ORIENTED_EDGE('',*,*,#5254,.T.) ;
#7500 = ORIENTED_EDGE('',*,*,#5252,.T.) ;
#7501 = ORIENTED_EDGE('',*,*,#5255,.F.) ;
#7502 = ORIENTED_EDGE('',*,*,#5256,.T.) ;
#7503 = ORIENTED_EDGE('',*,*,#5257,.F.) ;
#7504 = ORIENTED_EDGE('',*,*,#5256,.F.) ;
#7505 = ORIENTED_EDGE('',*,*,#5257,.T.) ;
#7506 = ORIENTED_EDGE('',*,*,#5255,.T.) ;
#7507 = ORIENTED_EDGE('',*,*,#5258,.F.) ;
#7508 = ORIENTED_EDGE('',*,*,#5259,.T.) ;
#7509 = ORIENTED_EDGE('',*,*,#5260,.F.) ;
#7510 = ORIENTED_EDGE('',*,*,#5259,.F.) ;
#7511 = ORIENTED_EDGE('',*,*,#5260,.T.) ;
#7512 = ORIENTED_EDGE('',*,*,#5258,.T.) ;
#7513 = ORIENTED_EDGE('',*,*,#5261,.F.) ;
#7514 = ORIENTED_EDGE('',*,*,#5262,.T.) ;
#7515 = ORIENTED_EDGE('',*,*,#5263,.F.) ;
#7516 = ORIENTED_EDGE('',*,*,#5262,.F.) ;
#7517 = ORIENTED_EDGE('',*,*,#5261,.T.) ;
#7518 = ORIENTED_EDGE('',*,*,#5264,.F.) ;
#7519 = ORIENTED_EDGE('',*,*,#5265,.T.) ;
#7520 = ORIENTED_EDGE('',*,*,#5266,.F.) ;
#7521 = ORIENTED_EDGE('',*,*,#5265,.F.) ;
#7522 = ORIENTED_EDGE('',*,*,#5266,.T.) ;
#7523 = ORIENTED_EDGE('',*,*,#5264,.T.) ;
#7524 = ORIENTED_EDGE('',*,*,#5263,.T.) ;
#7525 = ORIENTED_EDGE('',*,*,#5267,.F.) ;
#7526 = ORIENTED_EDGE('',*,*,#5268,.T.) ;
#7527 = ORIENTED_EDGE('',*,*,#5269,.F.) ;
#7528 = ORIENTED_EDGE('',*,*,#5268,.F.) ;
#7529 = ORIENTED_EDGE('',*,*,#5267,.T.) ;
#7530 = ORIENTED_EDGE('',*,*,#5270,.F.) ;
#7531 = ORIENTED_EDGE('',*,*,#5271,.T.) ;
#7532 = ORIENTED_EDGE('',*,*,#5272,.F.) ;
#7533 = ORIENTED_EDGE('',*,*,#5271,.F.) ;
#7534 = ORIENTED_EDGE('',*,*,#5272,.T.) ;
#7535 = ORIENTED_EDGE('',*,*,#5270,.T.) ;
#7536 = ORIENTED_EDGE('',*,*,#5269,.T.) ;
#7537 = PLANE('',#8685) ;
#7538 = PLANE('',#8686) ;
#7539 = PLANE('',#8687) ;
#7540 = PLANE('',#8688) ;
#7541 = PLANE('',#8689) ;
#7542 = PLANE('',#8690) ;
#7543 = PLANE('',#8698) ;
#7544 = PLANE('',#8702) ;
#7545 = PLANE('',#8706) ;
#7546 = PLANE('',#8707) ;
#7547 = PLANE('',#8708) ;
#7548 = PLANE('',#8709) ;
#7549 = PLANE('',#8710) ;
#7550 = PLANE('',#8714) ;
#7551 = PLANE('',#8715) ;
#7552 = PLANE('',#8716) ;
#7553 = PLANE('',#8717) ;
#7554 = PLANE('',#8718) ;
#7555 = PLANE('',#8724) ;
#7556 = PLANE('',#8725) ;
#7557 = PLANE('',#8731) ;
#7558 = PLANE('',#8737) ;
#7559 = PLANE('',#8738) ;
#7560 = PLANE('',#8745) ;
#7561 = PLANE('',#8746) ;
#7562 = PLANE('',#8747) ;
#7563 = PLANE('',#8748) ;
#7564 = PLANE('',#8749) ;
#7565 = PLANE('',#8750) ;
#7566 = PLANE('',#8751) ;
#7567 = PLANE('',#8752) ;
#7568 = PLANE('',#8753) ;
#7569 = PLANE('',#8754) ;
#7570 = PLANE('',#8757) ;
#7571 = PLANE('',#8758) ;
#7572 = PLANE('',#8759) ;
#7573 = PLANE('',#8760) ;
#7574 = PLANE('',#8761) ;
#7575 = PLANE('',#8762) ;
#7576 = PLANE('',#8763) ;
#7577 = PLANE('',#8768) ;
#7578 = PLANE('',#8773) ;
#7579 = PLANE('',#8775) ;
#7580 = PLANE('',#8784) ;
#7581 = PLANE('',#8786) ;
#7582 = PLANE('',#8787) ;
#7583 = PLANE('',#8788) ;
#7584 = PLANE('',#8793) ;
#7585 = PLANE('',#8794) ;
#7586 = PLANE('',#8795) ;
#7587 = PLANE('',#8803) ;
#7588 = PLANE('',#8804) ;
#7589 = PLANE('',#8805) ;
#7590 = PLANE('',#8806) ;
#7591 = PLANE('',#8807) ;
#7592 = PLANE('',#8808) ;
#7593 = PLANE('',#8809) ;
#7594 = PLANE('',#8810) ;
#7595 = PLANE('',#8811) ;
#7596 = PLANE('',#8812) ;
#7597 = PLANE('',#8813) ;
#7598 = PLANE('',#8814) ;
#7599 = PLANE('',#8815) ;
#7600 = PLANE('',#8816) ;
#7601 = PLANE('',#8817) ;
#7602 = PLANE('',#8818) ;
#7603 = PLANE('',#8825) ;
#7604 = PLANE('',#8826) ;
#7605 = PLANE('',#8833) ;
#7606 = PLANE('',#8834) ;
#7607 = PLANE('',#8838) ;
#7608 = PLANE('',#8839) ;
#7609 = PLANE('',#8847) ;
#7610 = PLANE('',#8848) ;
#7611 = PLANE('',#8856) ;
#7612 = PLANE('',#8857) ;
#7613 = PLANE('',#8864) ;
#7614 = PLANE('',#8877) ;
#7615 = PLANE('',#8881) ;
#7616 = PLANE('',#8882) ;
#7617 = PLANE('',#8887) ;
#7618 = PLANE('',#8891) ;
#7619 = PLANE('',#8892) ;
#7620 = PLANE('',#8897) ;
#7621 = PLANE('',#8898) ;
#7622 = PLANE('',#8900) ;
#7623 = PLANE('',#8901) ;
#7624 = PLANE('',#8903) ;
#7625 = PLANE('',#8904) ;
#7626 = PLANE('',#8906) ;
#7627 = PLANE('',#8908) ;
#7628 = PLANE('',#8910) ;
#7629 = PLANE('',#8911) ;
#7630 = PLANE('',#8915) ;
#7631 = PLANE('',#8926) ;
#7632 = PLANE('',#8927) ;
#7633 = PLANE('',#8931) ;
#7634 = PLANE('',#8941) ;
#7635 = PLANE('',#8950) ;
#7636 = PLANE('',#8974) ;
#7637 = PLANE('',#8975) ;
#7638 = PLANE('',#8983) ;
#7639 = PLANE('',#8987) ;
#7640 = PLANE('',#8988) ;
#7641 = PLANE('',#8993) ;
#7642 = PLANE('',#8994) ;
#7643 = PLANE('',#8999) ;
#7644 = PLANE('',#9000) ;
#7645 = PLANE('',#9015) ;
#7646 = PLANE('',#9016) ;
#7647 = PLANE('',#9017) ;
#7648 = PLANE('',#9018) ;
#7649 = PLANE('',#9022) ;
#7650 = PLANE('',#9029) ;
#7651 = PLANE('',#9030) ;
#7652 = PLANE('',#9031) ;
#7653 = PLANE('',#9032) ;
#7654 = PLANE('',#9033) ;
#7655 = PLANE('',#9035) ;
#7656 = PLANE('',#9040) ;
#7657 = PLANE('',#9043) ;
#7658 = PLANE('',#9207) ;
#7659 = PLANE('',#9318) ;
#7660 = PLANE('',#9320) ;
#7661 = PLANE('',#9323) ;
#7662 = PLANE('',#9331) ;
#7663 = PLANE('',#9332) ;
#7664 = PLANE('',#9334) ;
#7665 = PLANE('',#9335) ;
#7666 = PLANE('',#9336) ;
#7667 = PLANE('',#9337) ;
#7668 = PLANE('',#9338) ;
#7669 = PLANE('',#9342) ;
#7670 = PLANE('',#9343) ;
#7671 = PLANE('',#9344) ;
#7672 = PLANE('',#9345) ;
#7673 = PLANE('',#9346) ;
#7674 = PLANE('',#9347) ;
#7675 = PLANE('',#9348) ;
#7676 = PLANE('',#9448) ;
#7677 = PLANE('',#9513) ;
#7678 = PLANE('',#9518) ;
#7679 = PLANE('',#9519) ;
#7680 = PLANE('',#9520) ;
#7681 = PLANE('',#9521) ;
#7682 = PLANE('',#9522) ;
#7683 = PLANE('',#9523) ;
#7684 = PLANE('',#9524) ;
#7685 = PLANE('',#9529) ;
#7686 = PLANE('',#9530) ;
#7687 = PLANE('',#9534) ;
#7688 = PLANE('',#9535) ;
#7689 = PLANE('',#9540) ;
#7690 = PLANE('',#9541) ;
#7691 = PLANE('',#9546) ;
#7692 = PLANE('',#9547) ;
#7693 = PLANE('',#9679) ;
#7694 = PLANE('',#9767) ;
#7695 = PLANE('',#9784) ;
#7696 = PLANE('',#9785) ;
#7697 = PLANE('',#9786) ;
#7698 = PLANE('',#9787) ;
#7699 = PLANE('',#9788) ;
#7700 = PLANE('',#9789) ;
#7701 = PLANE('',#9790) ;
#7702 = PLANE('',#9791) ;
#7703 = PLANE('',#9792) ;
#7704 = PLANE('',#9793) ;
#7705 = PLANE('',#9795) ;
#7706 = PLANE('',#9796) ;
#7707 = PLANE('',#9797) ;
#7708 = PLANE('',#9798) ;
#7709 = PLANE('',#9799) ;
#7710 = PLANE('',#9803) ;
#7711 = PLANE('',#9804) ;
#7712 = PLANE('',#9805) ;
#7713 = PLANE('',#9806) ;
#7714 = PLANE('',#9807) ;
#7715 = PLANE('',#9808) ;
#7716 = PLANE('',#9817) ;
#7717 = PLANE('',#9821) ;
#7718 = PLANE('',#9822) ;
#7719 = PLANE('',#9826) ;
#7720 = PLANE('',#9827) ;
#7721 = PLANE('',#9832) ;
#7722 = PLANE('',#9833) ;
#7723 = PLANE('',#9837) ;
#7724 = PLANE('',#9838) ;
#7725 = PLANE('',#9842) ;
#7726 = PLANE('',#9843) ;
#7727 = PLANE('',#9845) ;
#7728 = PLANE('',#9848) ;
#7729 = PLANE('',#9849) ;
#7730 = PLANE('',#9850) ;
#7731 = PLANE('',#9853) ;
#7732 = PLANE('',#9854) ;
#7733 = PLANE('',#9855) ;
#7734 = PLANE('',#9859) ;
#7735 = PLANE('',#9860) ;
#7736 = PLANE('',#9861) ;
#7737 = PLANE('',#9862) ;
#7738 = PLANE('',#9867) ;
#7739 = PLANE('',#9868) ;
#7740 = PLANE('',#9872) ;
#7741 = PLANE('',#9873) ;
#7742 = PLANE('',#9877) ;
#7743 = PLANE('',#9878) ;
#7744 = PLANE('',#9883) ;
#7745 = PLANE('',#9884) ;
#7746 = PLANE('',#9899) ;
#7747 = PLANE('',#9903) ;
#7748 = PLANE('',#9904) ;
#7749 = PLANE('',#9909) ;
#7750 = PLANE('',#9913) ;
#7751 = PLANE('',#9914) ;
#7752 = ADVANCED_FACE('',(#1365),#7537,.T.) ;
#7753 = ADVANCED_FACE('',(#1366),#7538,.T.) ;
#7754 = ADVANCED_FACE('',(#1367),#7539,.T.) ;
#7755 = ADVANCED_FACE('',(#1368),#7540,.T.) ;
#7756 = ADVANCED_FACE('',(#1369),#7541,.T.) ;
#7757 = ADVANCED_FACE('',(#1370,#810,#811,#812,#813,#814,#815),#7542,.T.) ;
#7758 = ADVANCED_FACE('',(#1371),#626,.F.) ;
#7759 = ADVANCED_FACE('',(#1372),#7543,.F.) ;
#7760 = ADVANCED_FACE('',(#1373),#627,.F.) ;
#7761 = ADVANCED_FACE('',(#1374),#7544,.F.) ;
#7762 = ADVANCED_FACE('',(#1375),#628,.F.) ;
#7763 = ADVANCED_FACE('',(#1376,#816),#7545,.T.) ;
#7764 = ADVANCED_FACE('',(#1377),#7546,.F.) ;
#7765 = ADVANCED_FACE('',(#1378),#7547,.F.) ;
#7766 = ADVANCED_FACE('',(#1379),#7548,.F.) ;
#7767 = ADVANCED_FACE('',(#1380),#7549,.F.) ;
#7768 = ADVANCED_FACE('',(#1381),#629,.F.) ;
#7769 = ADVANCED_FACE('',(#1382,#817),#7550,.T.) ;
#7770 = ADVANCED_FACE('',(#1383),#7551,.F.) ;
#7771 = ADVANCED_FACE('',(#1384),#7552,.F.) ;
#7772 = ADVANCED_FACE('',(#1385),#7553,.F.) ;
#7773 = ADVANCED_FACE('',(#1386),#7554,.F.) ;
#7774 = ADVANCED_FACE('',(#1387),#630,.F.) ;
#7775 = ADVANCED_FACE('',(#1388),#631,.T.) ;
#7776 = ADVANCED_FACE('',(#1389,#818),#7555,.T.) ;
#7777 = ADVANCED_FACE('',(#1390),#7556,.T.) ;
#7778 = ADVANCED_FACE('',(#1391),#632,.F.) ;
#7779 = ADVANCED_FACE('',(#1392),#633,.T.) ;
#7780 = ADVANCED_FACE('',(#1393,#819),#7557,.T.) ;
#7781 = ADVANCED_FACE('',(#1394),#634,.F.) ;
#7782 = ADVANCED_FACE('',(#1395),#635,.T.) ;
#7783 = ADVANCED_FACE('',(#1396,#820),#7558,.T.) ;
#7784 = ADVANCED_FACE('',(#1397),#7559,.T.) ;
#7785 = ADVANCED_FACE('',(#1398),#636,.F.) ;
#7786 = ADVANCED_FACE('',(#1399),#637,.F.) ;
#7787 = ADVANCED_FACE('',(#1400),#7560,.T.) ;
#7788 = ADVANCED_FACE('',(#1401,#821),#7561,.F.) ;
#7789 = ADVANCED_FACE('',(#1402),#7562,.F.) ;
#7790 = ADVANCED_FACE('',(#1403,#822),#7563,.F.) ;
#7791 = ADVANCED_FACE('',(#1404),#7564,.F.) ;
#7792 = ADVANCED_FACE('',(#1405),#7565,.T.) ;
#7793 = ADVANCED_FACE('',(#1406,#823),#7566,.F.) ;
#7794 = ADVANCED_FACE('',(#1407),#7567,.F.) ;
#7795 = ADVANCED_FACE('',(#1408,#824),#7568,.F.) ;
#7796 = ADVANCED_FACE('',(#1409),#7569,.F.) ;
#7797 = ADVANCED_FACE('',(#1410),#638,.F.) ;
#7798 = ADVANCED_FACE('',(#1411),#7570,.T.) ;
#7799 = ADVANCED_FACE('',(#1412),#7571,.T.) ;
#7800 = ADVANCED_FACE('',(#1413),#7572,.T.) ;
#7801 = ADVANCED_FACE('',(#1414,#825),#7573,.T.) ;
#7802 = ADVANCED_FACE('',(#1415,#826,#827,#828,#829,#830),#7574,.F.) ;
#7803 = ADVANCED_FACE('',(#1416),#7575,.F.) ;
#7804 = ADVANCED_FACE('',(#1417),#7576,.F.) ;
#7805 = ADVANCED_FACE('',(#1418),#639,.F.) ;
#7806 = ADVANCED_FACE('',(#1419,#831),#7577,.F.) ;
#7807 = ADVANCED_FACE('',(#1420),#640,.F.) ;
#7808 = ADVANCED_FACE('',(#1421,#832),#7578,.F.) ;
#7809 = ADVANCED_FACE('',(#1422),#7579,.F.) ;
#7810 = ADVANCED_FACE('',(#1423),#641,.F.) ;
#7811 = ADVANCED_FACE('',(#1424),#642,.F.) ;
#7812 = ADVANCED_FACE('',(#1425),#643,.F.) ;
#7813 = ADVANCED_FACE('',(#1426,#833),#7580,.F.) ;
#7814 = ADVANCED_FACE('',(#1427),#7581,.F.) ;
#7815 = ADVANCED_FACE('',(#1428),#7582,.F.) ;
#7816 = ADVANCED_FACE('',(#1429),#7583,.F.) ;
#7817 = ADVANCED_FACE('',(#1430),#644,.F.) ;
#7818 = ADVANCED_FACE('',(#1431),#645,.F.) ;
#7819 = ADVANCED_FACE('',(#1432,#834,#835),#7584,.T.) ;
#7820 = ADVANCED_FACE('',(#1433),#7585,.F.) ;
#7821 = ADVANCED_FACE('',(#1434,#836),#7586,.F.) ;
#7822 = ADVANCED_FACE('',(#1435),#646,.F.) ;
#7823 = ADVANCED_FACE('',(#1436),#7587,.F.) ;
#7824 = ADVANCED_FACE('',(#1437),#7588,.T.) ;
#7825 = ADVANCED_FACE('',(#1438),#7589,.T.) ;
#7826 = ADVANCED_FACE('',(#1439),#7590,.T.) ;
#7827 = ADVANCED_FACE('',(#1440),#7591,.T.) ;
#7828 = ADVANCED_FACE('',(#1441),#7592,.T.) ;
#7829 = ADVANCED_FACE('',(#1442),#7593,.T.) ;
#7830 = ADVANCED_FACE('',(#1443),#7594,.T.) ;
#7831 = ADVANCED_FACE('',(#1444),#7595,.T.) ;
#7832 = ADVANCED_FACE('',(#1445),#7596,.T.) ;
#7833 = ADVANCED_FACE('',(#1446),#7597,.T.) ;
#7834 = ADVANCED_FACE('',(#1447),#7598,.T.) ;
#7835 = ADVANCED_FACE('',(#1448),#7599,.T.) ;
#7836 = ADVANCED_FACE('',(#1449),#7600,.T.) ;
#7837 = ADVANCED_FACE('',(#1450),#7601,.T.) ;
#7838 = ADVANCED_FACE('',(#1451),#7602,.T.) ;
#7839 = ADVANCED_FACE('',(#1452),#647,.T.) ;
#7840 = ADVANCED_FACE('',(#1453),#648,.F.) ;
#7841 = ADVANCED_FACE('',(#1454,#837),#7603,.F.) ;
#7842 = ADVANCED_FACE('',(#1455,#838),#7604,.T.) ;
#7843 = ADVANCED_FACE('',(#1456),#649,.T.) ;
#7844 = ADVANCED_FACE('',(#1457),#650,.F.) ;
#7845 = ADVANCED_FACE('',(#1458,#839),#7605,.F.) ;
#7846 = ADVANCED_FACE('',(#1459,#840),#7606,.T.) ;
#7847 = ADVANCED_FACE('',(#1460),#651,.T.) ;
#7848 = ADVANCED_FACE('',(#1461,#841),#7607,.T.) ;
#7849 = ADVANCED_FACE('',(#1462,#842,#843,#844),#7608,.T.) ;
#7850 = ADVANCED_FACE('',(#1463),#652,.F.) ;
#7851 = ADVANCED_FACE('',(#1464),#653,.T.) ;
#7852 = ADVANCED_FACE('',(#1465,#845),#7609,.T.) ;
#7853 = ADVANCED_FACE('',(#1466,#846),#7610,.T.) ;
#7854 = ADVANCED_FACE('',(#1467),#654,.F.) ;
#7855 = ADVANCED_FACE('',(#1468),#655,.T.) ;
#7856 = ADVANCED_FACE('',(#1469,#847),#7611,.T.) ;
#7857 = ADVANCED_FACE('',(#1470,#848),#7612,.T.) ;
#7858 = ADVANCED_FACE('',(#1471),#192,.T.) ;
#7859 = ADVANCED_FACE('',(#1472),#656,.T.) ;
#7860 = ADVANCED_FACE('',(#1473),#7613,.T.) ;
#7861 = ADVANCED_FACE('',(#1474),#657,.F.) ;
#7862 = ADVANCED_FACE('',(#1475),#658,.F.) ;
#7863 = ADVANCED_FACE('',(#1476,#849),#7614,.T.) ;
#7864 = ADVANCED_FACE('',(#1477),#659,.T.) ;
#7865 = ADVANCED_FACE('',(#1478,#850),#7615,.T.) ;
#7866 = ADVANCED_FACE('',(#1479,#851),#7616,.T.) ;
#7867 = ADVANCED_FACE('',(#1480),#660,.T.) ;
#7868 = ADVANCED_FACE('',(#1481),#7617,.T.) ;
#7869 = ADVANCED_FACE('',(#1482),#661,.T.) ;
#7870 = ADVANCED_FACE('',(#1483),#7618,.T.) ;
#7871 = ADVANCED_FACE('',(#1484,#852),#7619,.T.) ;
#7872 = ADVANCED_FACE('',(#1485),#662,.T.) ;
#7873 = ADVANCED_FACE('',(#1486),#7620,.T.) ;
#7874 = ADVANCED_FACE('',(#1487),#7621,.T.) ;
#7875 = ADVANCED_FACE('',(#1488),#7622,.F.) ;
#7876 = ADVANCED_FACE('',(#1489),#7623,.T.) ;
#7877 = ADVANCED_FACE('',(#1490),#7624,.F.) ;
#7878 = ADVANCED_FACE('',(#1491),#7625,.F.) ;
#7879 = ADVANCED_FACE('',(#1492),#7626,.F.) ;
#7880 = ADVANCED_FACE('',(#1493),#7627,.T.) ;
#7881 = ADVANCED_FACE('',(#1494),#7628,.F.) ;
#7882 = ADVANCED_FACE('',(#1495),#7629,.F.) ;
#7883 = ADVANCED_FACE('',(#1496),#663,.F.) ;
#7884 = ADVANCED_FACE('',(#1497),#7630,.F.) ;
#7885 = ADVANCED_FACE('',(#1498),#664,.F.) ;
#7886 = ADVANCED_FACE('',(#1499,#853),#665,.F.) ;
#7887 = ADVANCED_FACE('',(#1500,#854),#7631,.T.) ;
#7888 = ADVANCED_FACE('',(#1501,#855,#856),#7632,.T.) ;
#7889 = ADVANCED_FACE('',(#1502,#857),#666,.T.) ;
#7890 = ADVANCED_FACE('',(#1503,#858),#7633,.T.) ;
#7891 = ADVANCED_FACE('',(#1504),#193,.F.) ;
#7892 = ADVANCED_FACE('',(#1505),#194,.T.) ;
#7893 = ADVANCED_FACE('',(#1506),#667,.F.) ;
#7894 = ADVANCED_FACE('',(#1507),#668,.F.) ;
#7895 = ADVANCED_FACE('',(#1508,#859),#7634,.T.) ;
#7896 = ADVANCED_FACE('',(#1509),#669,.T.) ;
#7897 = ADVANCED_FACE('',(#1510),#670,.T.) ;
#7898 = ADVANCED_FACE('',(#1511,#860),#7635,.T.) ;
#7899 = ADVANCED_FACE('',(#1512),#671,.T.) ;
#7900 = ADVANCED_FACE('',(#1513),#672,.T.) ;
#7901 = ADVANCED_FACE('',(#1514),#673,.F.) ;
#7902 = ADVANCED_FACE('',(#1515),#674,.F.) ;
#7903 = ADVANCED_FACE('',(#1516),#195,.T.) ;
#7904 = ADVANCED_FACE('',(#1517),#196,.T.) ;
#7905 = ADVANCED_FACE('',(#1518),#197,.T.) ;
#7906 = ADVANCED_FACE('',(#1519),#675,.F.) ;
#7907 = ADVANCED_FACE('',(#1520),#676,.T.) ;
#7908 = ADVANCED_FACE('',(#1521,#861),#7636,.T.) ;
#7909 = ADVANCED_FACE('',(#1522,#862),#7637,.T.) ;
#7910 = ADVANCED_FACE('',(#1523),#677,.F.) ;
#7911 = ADVANCED_FACE('',(#1524),#678,.F.) ;
#7912 = ADVANCED_FACE('',(#1525,#863),#7638,.T.) ;
#7913 = ADVANCED_FACE('',(#1526),#679,.T.) ;
#7914 = ADVANCED_FACE('',(#1527,#864),#7639,.T.) ;
#7915 = ADVANCED_FACE('',(#1528,#865),#7640,.T.) ;
#7916 = ADVANCED_FACE('',(#1529),#680,.T.) ;
#7917 = ADVANCED_FACE('',(#1530),#7641,.T.) ;
#7918 = ADVANCED_FACE('',(#1531),#7642,.T.) ;
#7919 = ADVANCED_FACE('',(#1532),#681,.T.) ;
#7920 = ADVANCED_FACE('',(#1533),#7643,.T.) ;
#7921 = ADVANCED_FACE('',(#1534),#7644,.T.) ;
#7922 = ADVANCED_FACE('',(#1535),#682,.F.) ;
#7923 = ADVANCED_FACE('',(#1536),#7645,.F.) ;
#7924 = ADVANCED_FACE('',(#1537),#7646,.F.) ;
#7925 = ADVANCED_FACE('',(#1538),#7647,.F.) ;
#7926 = ADVANCED_FACE('',(#1539,#866),#7648,.F.) ;
#7927 = ADVANCED_FACE('',(#1540),#7649,.F.) ;
#7928 = ADVANCED_FACE('',(#1541),#683,.F.) ;
#7929 = ADVANCED_FACE('',(#1542),#684,.T.) ;
#7930 = ADVANCED_FACE('',(#1543),#685,.T.) ;
#7931 = ADVANCED_FACE('',(#1544,#867),#7650,.T.) ;
#7932 = ADVANCED_FACE('',(#1545),#7651,.T.) ;
#7933 = ADVANCED_FACE('',(#1546,#868),#7652,.F.) ;
#7934 = ADVANCED_FACE('',(#1547,#869),#7653,.F.) ;
#7935 = ADVANCED_FACE('',(#1548),#7654,.F.) ;
#7936 = ADVANCED_FACE('',(#1549,#870),#7655,.T.) ;
#7937 = ADVANCED_FACE('',(#1550),#686,.T.) ;
#7938 = ADVANCED_FACE('',(#1551),#7656,.T.) ;
#7939 = ADVANCED_FACE('',(#1552),#687,.T.) ;
#7940 = ADVANCED_FACE('',(#1553),#7657,.T.) ;
#7941 = ADVANCED_FACE('',(#1554),#198,.T.) ;
#7942 = ADVANCED_FACE('',(#1555),#199,.T.) ;
#7943 = ADVANCED_FACE('',(#1556),#200,.T.) ;
#7944 = ADVANCED_FACE('',(#1557),#201,.T.) ;
#7945 = ADVANCED_FACE('',(#1558),#202,.T.) ;
#7946 = ADVANCED_FACE('',(#1559),#203,.T.) ;
#7947 = ADVANCED_FACE('',(#1560),#204,.T.) ;
#7948 = ADVANCED_FACE('',(#1561),#205,.T.) ;
#7949 = ADVANCED_FACE('',(#1562),#206,.T.) ;
#7950 = ADVANCED_FACE('',(#1563),#207,.T.) ;
#7951 = ADVANCED_FACE('',(#1564),#208,.T.) ;
#7952 = ADVANCED_FACE('',(#1565),#209,.T.) ;
#7953 = ADVANCED_FACE('',(#1566),#210,.T.) ;
#7954 = ADVANCED_FACE('',(#1567),#211,.T.) ;
#7955 = ADVANCED_FACE('',(#1568),#212,.T.) ;
#7956 = ADVANCED_FACE('',(#1569),#213,.T.) ;
#7957 = ADVANCED_FACE('',(#1570),#214,.T.) ;
#7958 = ADVANCED_FACE('',(#1571),#215,.T.) ;
#7959 = ADVANCED_FACE('',(#1572),#216,.T.) ;
#7960 = ADVANCED_FACE('',(#1573),#217,.T.) ;
#7961 = ADVANCED_FACE('',(#1574),#218,.T.) ;
#7962 = ADVANCED_FACE('',(#1575),#219,.T.) ;
#7963 = ADVANCED_FACE('',(#1576),#220,.T.) ;
#7964 = ADVANCED_FACE('',(#1577),#221,.T.) ;
#7965 = ADVANCED_FACE('',(#1578),#222,.T.) ;
#7966 = ADVANCED_FACE('',(#1579),#223,.T.) ;
#7967 = ADVANCED_FACE('',(#1580),#224,.T.) ;
#7968 = ADVANCED_FACE('',(#1581),#225,.T.) ;
#7969 = ADVANCED_FACE('',(#1582),#226,.T.) ;
#7970 = ADVANCED_FACE('',(#1583),#227,.T.) ;
#7971 = ADVANCED_FACE('',(#1584),#228,.T.) ;
#7972 = ADVANCED_FACE('',(#1585),#229,.T.) ;
#7973 = ADVANCED_FACE('',(#1586),#230,.T.) ;
#7974 = ADVANCED_FACE('',(#1587),#231,.T.) ;
#7975 = ADVANCED_FACE('',(#1588),#232,.T.) ;
#7976 = ADVANCED_FACE('',(#1589),#233,.T.) ;
#7977 = ADVANCED_FACE('',(#1590),#234,.T.) ;
#7978 = ADVANCED_FACE('',(#1591),#235,.T.) ;
#7979 = ADVANCED_FACE('',(#1592),#236,.T.) ;
#7980 = ADVANCED_FACE('',(#1593),#688,.T.) ;
#7981 = ADVANCED_FACE('',(#1594),#7658,.T.) ;
#7982 = ADVANCED_FACE('',(#1595),#689,.T.) ;
#7983 = ADVANCED_FACE('',(#1596),#690,.T.) ;
#7984 = ADVANCED_FACE('',(#1597),#691,.T.) ;
#7985 = ADVANCED_FACE('',(#1598),#692,.T.) ;
#7986 = ADVANCED_FACE('',(#1599),#693,.T.) ;
#7987 = ADVANCED_FACE('',(#1600),#694,.T.) ;
#7988 = ADVANCED_FACE('',(#1601),#695,.T.) ;
#7989 = ADVANCED_FACE('',(#1602),#696,.T.) ;
#7990 = ADVANCED_FACE('',(#1603),#697,.T.) ;
#7991 = ADVANCED_FACE('',(#1604),#698,.T.) ;
#7992 = ADVANCED_FACE('',(#1605),#699,.T.) ;
#7993 = ADVANCED_FACE('',(#1606),#700,.T.) ;
#7994 = ADVANCED_FACE('',(#1607),#701,.T.) ;
#7995 = ADVANCED_FACE('',(#1608),#702,.T.) ;
#7996 = ADVANCED_FACE('',(#1609),#703,.T.) ;
#7997 = ADVANCED_FACE('',(#1610),#704,.T.) ;
#7998 = ADVANCED_FACE('',(#1611),#705,.T.) ;
#7999 = ADVANCED_FACE('',(#1612),#706,.T.) ;
#8000 = ADVANCED_FACE('',(#1613),#707,.T.) ;
#8001 = ADVANCED_FACE('',(#1614),#708,.T.) ;
#8002 = ADVANCED_FACE('',(#1615),#709,.T.) ;
#8003 = ADVANCED_FACE('',(#1616),#710,.T.) ;
#8004 = ADVANCED_FACE('',(#1617),#711,.T.) ;
#8005 = ADVANCED_FACE('',(#1618),#712,.T.) ;
#8006 = ADVANCED_FACE('',(#1619),#713,.T.) ;
#8007 = ADVANCED_FACE('',(#1620),#714,.T.) ;
#8008 = ADVANCED_FACE('',(#1621),#715,.T.) ;
#8009 = ADVANCED_FACE('',(#1622),#716,.T.) ;
#8010 = ADVANCED_FACE('',(#1623),#717,.T.) ;
#8011 = ADVANCED_FACE('',(#1624),#718,.T.) ;
#8012 = ADVANCED_FACE('',(#1625),#719,.T.) ;
#8013 = ADVANCED_FACE('',(#1626),#720,.T.) ;
#8014 = ADVANCED_FACE('',(#1627),#721,.T.) ;
#8015 = ADVANCED_FACE('',(#1628),#722,.T.) ;
#8016 = ADVANCED_FACE('',(#1629),#723,.T.) ;
#8017 = ADVANCED_FACE('',(#1630),#724,.T.) ;
#8018 = ADVANCED_FACE('',(#1631),#725,.T.) ;
#8019 = ADVANCED_FACE('',(#1632),#726,.T.) ;
#8020 = ADVANCED_FACE('',(#1633),#727,.T.) ;
#8021 = ADVANCED_FACE('',(#1634),#7659,.T.) ;
#8022 = ADVANCED_FACE('',(#1635,#871),#7660,.T.) ;
#8023 = ADVANCED_FACE('',(#1636,#872),#7661,.T.) ;
#8024 = ADVANCED_FACE('',(#1637),#728,.T.) ;
#8025 = ADVANCED_FACE('',(#1638),#729,.T.) ;
#8026 = ADVANCED_FACE('',(#1639),#730,.T.) ;
#8027 = ADVANCED_FACE('',(#1640),#7662,.T.) ;
#8028 = ADVANCED_FACE('',(#1641),#7663,.T.) ;
#8029 = ADVANCED_FACE('',(#1642),#7664,.T.) ;
#8030 = ADVANCED_FACE('',(#1643),#7665,.F.) ;
#8031 = ADVANCED_FACE('',(#1644),#7666,.F.) ;
#8032 = ADVANCED_FACE('',(#1645),#7667,.F.) ;
#8033 = ADVANCED_FACE('',(#1646),#7668,.F.) ;
#8034 = ADVANCED_FACE('',(#1647),#731,.F.) ;
#8035 = ADVANCED_FACE('',(#1648),#7669,.F.) ;
#8036 = ADVANCED_FACE('',(#1649,#873),#7670,.T.) ;
#8037 = ADVANCED_FACE('',(#1650,#874),#7671,.F.) ;
#8038 = ADVANCED_FACE('',(#1651),#7672,.F.) ;
#8039 = ADVANCED_FACE('',(#1652),#7673,.F.) ;
#8040 = ADVANCED_FACE('',(#1653),#7674,.F.) ;
#8041 = ADVANCED_FACE('',(#1654),#7675,.F.) ;
#8042 = ADVANCED_FACE('',(#1655),#237,.T.) ;
#8043 = ADVANCED_FACE('',(#1656),#238,.T.) ;
#8044 = ADVANCED_FACE('',(#1657),#239,.T.) ;
#8045 = ADVANCED_FACE('',(#1658),#240,.T.) ;
#8046 = ADVANCED_FACE('',(#1659),#241,.T.) ;
#8047 = ADVANCED_FACE('',(#1660),#242,.T.) ;
#8048 = ADVANCED_FACE('',(#1661),#243,.T.) ;
#8049 = ADVANCED_FACE('',(#1662),#244,.T.) ;
#8050 = ADVANCED_FACE('',(#1663),#245,.T.) ;
#8051 = ADVANCED_FACE('',(#1664),#246,.T.) ;
#8052 = ADVANCED_FACE('',(#1665),#247,.T.) ;
#8053 = ADVANCED_FACE('',(#1666),#248,.T.) ;
#8054 = ADVANCED_FACE('',(#1667),#249,.T.) ;
#8055 = ADVANCED_FACE('',(#1668),#250,.T.) ;
#8056 = ADVANCED_FACE('',(#1669),#251,.T.) ;
#8057 = ADVANCED_FACE('',(#1670),#252,.T.) ;
#8058 = ADVANCED_FACE('',(#1671),#253,.T.) ;
#8059 = ADVANCED_FACE('',(#1672),#254,.T.) ;
#8060 = ADVANCED_FACE('',(#1673),#255,.T.) ;
#8061 = ADVANCED_FACE('',(#1674),#256,.T.) ;
#8062 = ADVANCED_FACE('',(#1675),#257,.T.) ;
#8063 = ADVANCED_FACE('',(#1676),#258,.T.) ;
#8064 = ADVANCED_FACE('',(#1677),#259,.T.) ;
#8065 = ADVANCED_FACE('',(#1678),#732,.T.) ;
#8066 = ADVANCED_FACE('',(#1679),#7676,.T.) ;
#8067 = ADVANCED_FACE('',(#1680),#733,.T.) ;
#8068 = ADVANCED_FACE('',(#1681),#734,.T.) ;
#8069 = ADVANCED_FACE('',(#1682),#735,.T.) ;
#8070 = ADVANCED_FACE('',(#1683),#736,.T.) ;
#8071 = ADVANCED_FACE('',(#1684),#737,.T.) ;
#8072 = ADVANCED_FACE('',(#1685),#738,.T.) ;
#8073 = ADVANCED_FACE('',(#1686),#739,.T.) ;
#8074 = ADVANCED_FACE('',(#1687),#740,.T.) ;
#8075 = ADVANCED_FACE('',(#1688),#741,.T.) ;
#8076 = ADVANCED_FACE('',(#1689),#742,.T.) ;
#8077 = ADVANCED_FACE('',(#1690),#743,.T.) ;
#8078 = ADVANCED_FACE('',(#1691),#744,.T.) ;
#8079 = ADVANCED_FACE('',(#1692),#745,.T.) ;
#8080 = ADVANCED_FACE('',(#1693),#746,.T.) ;
#8081 = ADVANCED_FACE('',(#1694),#747,.T.) ;
#8082 = ADVANCED_FACE('',(#1695),#748,.T.) ;
#8083 = ADVANCED_FACE('',(#1696),#749,.T.) ;
#8084 = ADVANCED_FACE('',(#1697),#750,.T.) ;
#8085 = ADVANCED_FACE('',(#1698),#751,.T.) ;
#8086 = ADVANCED_FACE('',(#1699),#752,.T.) ;
#8087 = ADVANCED_FACE('',(#1700),#753,.T.) ;
#8088 = ADVANCED_FACE('',(#1701),#754,.T.) ;
#8089 = ADVANCED_FACE('',(#1702),#755,.T.) ;
#8090 = ADVANCED_FACE('',(#1703),#7677,.T.) ;
#8091 = ADVANCED_FACE('',(#1704),#756,.T.) ;
#8092 = ADVANCED_FACE('',(#1705),#7678,.T.) ;
#8093 = ADVANCED_FACE('',(#1706,#875),#7679,.T.) ;
#8094 = ADVANCED_FACE('',(#1707),#7680,.F.) ;
#8095 = ADVANCED_FACE('',(#1708),#7681,.F.) ;
#8096 = ADVANCED_FACE('',(#1709),#7682,.F.) ;
#8097 = ADVANCED_FACE('',(#1710),#7683,.F.) ;
#8098 = ADVANCED_FACE('',(#1711),#7684,.F.) ;
#8099 = ADVANCED_FACE('',(#1712),#757,.T.) ;
#8100 = ADVANCED_FACE('',(#1713),#7685,.T.) ;
#8101 = ADVANCED_FACE('',(#1714),#7686,.T.) ;
#8102 = ADVANCED_FACE('',(#1715),#758,.T.) ;
#8103 = ADVANCED_FACE('',(#1716),#7687,.T.) ;
#8104 = ADVANCED_FACE('',(#1717),#7688,.T.) ;
#8105 = ADVANCED_FACE('',(#1718),#759,.T.) ;
#8106 = ADVANCED_FACE('',(#1719),#7689,.T.) ;
#8107 = ADVANCED_FACE('',(#1720),#7690,.T.) ;
#8108 = ADVANCED_FACE('',(#1721),#760,.T.) ;
#8109 = ADVANCED_FACE('',(#1722),#7691,.T.) ;
#8110 = ADVANCED_FACE('',(#1723),#7692,.T.) ;
#8111 = ADVANCED_FACE('',(#1724),#260,.T.) ;
#8112 = ADVANCED_FACE('',(#1725),#261,.T.) ;
#8113 = ADVANCED_FACE('',(#1726),#262,.T.) ;
#8114 = ADVANCED_FACE('',(#1727),#263,.T.) ;
#8115 = ADVANCED_FACE('',(#1728),#264,.T.) ;
#8116 = ADVANCED_FACE('',(#1729),#265,.T.) ;
#8117 = ADVANCED_FACE('',(#1730),#266,.T.) ;
#8118 = ADVANCED_FACE('',(#1731),#267,.T.) ;
#8119 = ADVANCED_FACE('',(#1732),#268,.T.) ;
#8120 = ADVANCED_FACE('',(#1733),#269,.T.) ;
#8121 = ADVANCED_FACE('',(#1734),#270,.T.) ;
#8122 = ADVANCED_FACE('',(#1735),#271,.T.) ;
#8123 = ADVANCED_FACE('',(#1736),#272,.T.) ;
#8124 = ADVANCED_FACE('',(#1737),#273,.T.) ;
#8125 = ADVANCED_FACE('',(#1738),#274,.T.) ;
#8126 = ADVANCED_FACE('',(#1739),#275,.T.) ;
#8127 = ADVANCED_FACE('',(#1740),#276,.T.) ;
#8128 = ADVANCED_FACE('',(#1741),#277,.T.) ;
#8129 = ADVANCED_FACE('',(#1742),#278,.T.) ;
#8130 = ADVANCED_FACE('',(#1743),#279,.T.) ;
#8131 = ADVANCED_FACE('',(#1744),#280,.T.) ;
#8132 = ADVANCED_FACE('',(#1745),#281,.T.) ;
#8133 = ADVANCED_FACE('',(#1746),#282,.T.) ;
#8134 = ADVANCED_FACE('',(#1747),#283,.T.) ;
#8135 = ADVANCED_FACE('',(#1748),#284,.T.) ;
#8136 = ADVANCED_FACE('',(#1749),#285,.T.) ;
#8137 = ADVANCED_FACE('',(#1750),#286,.T.) ;
#8138 = ADVANCED_FACE('',(#1751),#287,.T.) ;
#8139 = ADVANCED_FACE('',(#1752),#288,.T.) ;
#8140 = ADVANCED_FACE('',(#1753),#289,.T.) ;
#8141 = ADVANCED_FACE('',(#1754),#290,.T.) ;
#8142 = ADVANCED_FACE('',(#1755),#761,.T.) ;
#8143 = ADVANCED_FACE('',(#1756),#7693,.T.) ;
#8144 = ADVANCED_FACE('',(#1757),#762,.T.) ;
#8145 = ADVANCED_FACE('',(#1758),#763,.T.) ;
#8146 = ADVANCED_FACE('',(#1759),#764,.T.) ;
#8147 = ADVANCED_FACE('',(#1760),#765,.T.) ;
#8148 = ADVANCED_FACE('',(#1761),#766,.T.) ;
#8149 = ADVANCED_FACE('',(#1762),#767,.T.) ;
#8150 = ADVANCED_FACE('',(#1763),#768,.T.) ;
#8151 = ADVANCED_FACE('',(#1764),#769,.T.) ;
#8152 = ADVANCED_FACE('',(#1765),#770,.T.) ;
#8153 = ADVANCED_FACE('',(#1766),#771,.T.) ;
#8154 = ADVANCED_FACE('',(#1767),#772,.T.) ;
#8155 = ADVANCED_FACE('',(#1768),#773,.T.) ;
#8156 = ADVANCED_FACE('',(#1769),#774,.T.) ;
#8157 = ADVANCED_FACE('',(#1770),#775,.T.) ;
#8158 = ADVANCED_FACE('',(#1771),#776,.T.) ;
#8159 = ADVANCED_FACE('',(#1772),#777,.T.) ;
#8160 = ADVANCED_FACE('',(#1773),#778,.T.) ;
#8161 = ADVANCED_FACE('',(#1774),#779,.T.) ;
#8162 = ADVANCED_FACE('',(#1775),#780,.T.) ;
#8163 = ADVANCED_FACE('',(#1776),#781,.T.) ;
#8164 = ADVANCED_FACE('',(#1777),#782,.T.) ;
#8165 = ADVANCED_FACE('',(#1778),#783,.T.) ;
#8166 = ADVANCED_FACE('',(#1779),#784,.T.) ;
#8167 = ADVANCED_FACE('',(#1780),#785,.T.) ;
#8168 = ADVANCED_FACE('',(#1781),#786,.T.) ;
#8169 = ADVANCED_FACE('',(#1782),#787,.T.) ;
#8170 = ADVANCED_FACE('',(#1783),#788,.T.) ;
#8171 = ADVANCED_FACE('',(#1784),#789,.T.) ;
#8172 = ADVANCED_FACE('',(#1785),#790,.T.) ;
#8173 = ADVANCED_FACE('',(#1786),#791,.T.) ;
#8174 = ADVANCED_FACE('',(#1787),#792,.T.) ;
#8175 = ADVANCED_FACE('',(#1788),#7694,.T.) ;
#8176 = ADVANCED_FACE('',(#1789),#793,.F.) ;
#8177 = ADVANCED_FACE('',(#1790,#876),#7695,.F.) ;
#8178 = ADVANCED_FACE('',(#1791),#7696,.T.) ;
#8179 = ADVANCED_FACE('',(#1792,#877),#7697,.F.) ;
#8180 = ADVANCED_FACE('',(#1793),#7698,.F.) ;
#8181 = ADVANCED_FACE('',(#1794),#7699,.T.) ;
#8182 = ADVANCED_FACE('',(#1795),#7700,.T.) ;
#8183 = ADVANCED_FACE('',(#1796),#7701,.F.) ;
#8184 = ADVANCED_FACE('',(#1797),#7702,.F.) ;
#8185 = ADVANCED_FACE('',(#1798),#7703,.F.) ;
#8186 = ADVANCED_FACE('',(#1799),#7704,.F.) ;
#8187 = ADVANCED_FACE('',(#1800),#7705,.F.) ;
#8188 = ADVANCED_FACE('',(#1801),#7706,.T.) ;
#8189 = ADVANCED_FACE('',(#1802),#7707,.T.) ;
#8190 = ADVANCED_FACE('',(#1803),#7708,.T.) ;
#8191 = ADVANCED_FACE('',(#1804,#878),#7709,.T.) ;
#8192 = ADVANCED_FACE('',(#1805),#794,.F.) ;
#8193 = ADVANCED_FACE('',(#1806),#7710,.T.) ;
#8194 = ADVANCED_FACE('',(#1807),#7711,.F.) ;
#8195 = ADVANCED_FACE('',(#1808),#7712,.F.) ;
#8196 = ADVANCED_FACE('',(#1809,#879),#7713,.F.) ;
#8197 = ADVANCED_FACE('',(#1810),#7714,.F.) ;
#8198 = ADVANCED_FACE('',(#1811,#880),#7715,.F.) ;
#8199 = ADVANCED_FACE('',(#1812),#291,.T.) ;
#8200 = ADVANCED_FACE('',(#1813),#292,.T.) ;
#8201 = ADVANCED_FACE('',(#1814),#795,.T.) ;
#8202 = ADVANCED_FACE('',(#1815),#7716,.T.) ;
#8203 = ADVANCED_FACE('',(#1816),#796,.T.) ;
#8204 = ADVANCED_FACE('',(#1817),#7717,.T.) ;
#8205 = ADVANCED_FACE('',(#1818),#7718,.T.) ;
#8206 = ADVANCED_FACE('',(#1819),#797,.T.) ;
#8207 = ADVANCED_FACE('',(#1820),#7719,.T.) ;
#8208 = ADVANCED_FACE('',(#1821),#7720,.T.) ;
#8209 = ADVANCED_FACE('',(#1822),#798,.T.) ;
#8210 = ADVANCED_FACE('',(#1823),#7721,.T.) ;
#8211 = ADVANCED_FACE('',(#1824),#7722,.T.) ;
#8212 = ADVANCED_FACE('',(#1825),#799,.T.) ;
#8213 = ADVANCED_FACE('',(#1826),#7723,.T.) ;
#8214 = ADVANCED_FACE('',(#1827),#7724,.T.) ;
#8215 = ADVANCED_FACE('',(#1828),#800,.T.) ;
#8216 = ADVANCED_FACE('',(#1829),#7725,.T.) ;
#8217 = ADVANCED_FACE('',(#1830),#7726,.T.) ;
#8218 = ADVANCED_FACE('',(#1831),#7727,.T.) ;
#8219 = ADVANCED_FACE('',(#1832),#7728,.T.) ;
#8220 = ADVANCED_FACE('',(#1833),#7729,.T.) ;
#8221 = ADVANCED_FACE('',(#1834),#7730,.T.) ;
#8222 = ADVANCED_FACE('',(#1835),#7731,.F.) ;
#8223 = ADVANCED_FACE('',(#1836),#7732,.T.) ;
#8224 = ADVANCED_FACE('',(#1837),#7733,.T.) ;
#8225 = ADVANCED_FACE('',(#1838),#801,.F.) ;
#8226 = ADVANCED_FACE('',(#1839),#7734,.F.) ;
#8227 = ADVANCED_FACE('',(#1840),#7735,.F.) ;
#8228 = ADVANCED_FACE('',(#1841,#881),#7736,.F.) ;
#8229 = ADVANCED_FACE('',(#1842,#882),#7737,.F.) ;
#8230 = ADVANCED_FACE('',(#1843),#802,.T.) ;
#8231 = ADVANCED_FACE('',(#1844),#7738,.T.) ;
#8232 = ADVANCED_FACE('',(#1845),#7739,.T.) ;
#8233 = ADVANCED_FACE('',(#1846),#803,.T.) ;
#8234 = ADVANCED_FACE('',(#1847),#7740,.T.) ;
#8235 = ADVANCED_FACE('',(#1848),#7741,.T.) ;
#8236 = ADVANCED_FACE('',(#1849),#804,.T.) ;
#8237 = ADVANCED_FACE('',(#1850),#7742,.T.) ;
#8238 = ADVANCED_FACE('',(#1851),#7743,.T.) ;
#8239 = ADVANCED_FACE('',(#1852),#805,.T.) ;
#8240 = ADVANCED_FACE('',(#1853),#7744,.T.) ;
#8241 = ADVANCED_FACE('',(#1854),#7745,.T.) ;
#8242 = ADVANCED_FACE('',(#1855),#806,.T.) ;
#8243 = ADVANCED_FACE('',(#1856),#7746,.T.) ;
#8244 = ADVANCED_FACE('',(#1857),#807,.T.) ;
#8245 = ADVANCED_FACE('',(#1858),#7747,.T.) ;
#8246 = ADVANCED_FACE('',(#1859,#883),#7748,.T.) ;
#8247 = ADVANCED_FACE('',(#1860),#808,.T.) ;
#8248 = ADVANCED_FACE('',(#1861),#7749,.T.) ;
#8249 = ADVANCED_FACE('',(#1862),#809,.T.) ;
#8250 = ADVANCED_FACE('',(#1863),#7750,.T.) ;
#8251 = ADVANCED_FACE('',(#1864,#884),#7751,.T.) ;
#8252 = CLOSED_SHELL('',(#7752,#7753,#7754,#7755,#7756,#7757,#7758,#7759,
#7760,#7761,#7762,#7763,#7764,#7765,#7766,#7767,#7768,#7769,#7770,#7771,
#7772,#7773,#7774,#7775,#7776,#7777,#7778,#7779,#7780,#7781,#7782,#7783,
#7784,#7785,#7786,#7787,#7788,#7789,#7790,#7791,#7792,#7793,#7794,#7795,
#7796,#7797,#7798,#7799,#7800,#7801,#7802,#7803,#7804)) ;
#8253 = CLOSED_SHELL('',(#7805,#7806,#7807,#7808,#7809,#7810,#7811,#7812,
#7813,#7814,#7815,#7816,#7817,#7818,#7819,#7820,#7821)) ;
#8254 = CLOSED_SHELL('',(#7822,#7823,#7824,#7825,#7826,#7827,#7828,#7829,
#7830,#7831,#7832,#7833,#7834,#7835,#7836,#7837,#7838,#7839,#7840,#7841,
#7842,#7843,#7844,#7845,#7846,#7847,#7848,#7849)) ;
#8255 = CLOSED_SHELL('',(#7850,#7851,#7852,#7853)) ;
#8256 = CLOSED_SHELL('',(#7854,#7855,#7856,#7857)) ;
#8257 = CLOSED_SHELL('',(#7858,#7859,#7860)) ;
#8258 = CLOSED_SHELL('',(#7861,#7862,#7863,#7864,#7865,#7866)) ;
#8259 = CLOSED_SHELL('',(#7867,#7868,#7869,#7870,#7871)) ;
#8260 = CLOSED_SHELL('',(#7872,#7873,#7874)) ;
#8261 = CLOSED_SHELL('',(#7875,#7876,#7877,#7878,#7879,#7880,#7881,#7882,
#7883,#7884,#7885,#7886,#7887,#7888,#7889,#7890)) ;
#8262 = CLOSED_SHELL('',(#7891)) ;
#8263 = CLOSED_SHELL('',(#7892,#7893,#7894)) ;
#8264 = CLOSED_SHELL('',(#7895,#7896,#7897,#7898,#7899,#7900,#7901,#7902,
#7903,#7904,#7905)) ;
#8265 = CLOSED_SHELL('',(#7906,#7907,#7908,#7909)) ;
#8266 = CLOSED_SHELL('',(#7910,#7911,#7912,#7913,#7914,#7915)) ;
#8267 = CLOSED_SHELL('',(#7916,#7917,#7918)) ;
#8268 = CLOSED_SHELL('',(#7919,#7920,#7921)) ;
#8269 = CLOSED_SHELL('',(#7922,#7923,#7924,#7925,#7926,#7927,#7928,#7929,
#7930,#7931,#7932,#7933,#7934,#7935)) ;
#8270 = CLOSED_SHELL('',(#7936,#7937,#7938,#7939,#7940)) ;
#8271 = CLOSED_SHELL('',(#7941,#7942,#7943,#7944,#7945,#7946,#7947,#7948,
#7949,#7950,#7951,#7952,#7953,#7954,#7955,#7956,#7957,#7958,#7959,#7960,
#7961,#7962,#7963,#7964,#7965,#7966,#7967,#7968,#7969,#7970,#7971,#7972,
#7973,#7974,#7975,#7976,#7977,#7978,#7979,#7980,#7981,#7982,#7983,#7984,
#7985,#7986,#7987,#7988,#7989,#7990,#7991,#7992,#7993,#7994,#7995,#7996,
#7997,#7998,#7999,#8000,#8001,#8002,#8003,#8004,#8005,#8006,#8007,#8008,
#8009,#8010,#8011,#8012,#8013,#8014,#8015,#8016,#8017,#8018,#8019,#8020,
#8021)) ;
#8272 = CLOSED_SHELL('',(#8022,#8023,#8024,#8025,#8026,#8027,#8028)) ;
#8273 = CLOSED_SHELL('',(#8029,#8030,#8031,#8032,#8033,#8034,#8035,#8036,
#8037,#8038,#8039,#8040,#8041)) ;
#8274 = CLOSED_SHELL('',(#8042,#8043,#8044,#8045,#8046,#8047,#8048,#8049,
#8050,#8051,#8052,#8053,#8054,#8055,#8056,#8057,#8058,#8059,#8060,#8061,
#8062,#8063,#8064,#8065,#8066,#8067,#8068,#8069,#8070,#8071,#8072,#8073,
#8074,#8075,#8076,#8077,#8078,#8079,#8080,#8081,#8082,#8083,#8084,#8085,
#8086,#8087,#8088,#8089,#8090)) ;
#8275 = CLOSED_SHELL('',(#8091,#8092,#8093,#8094,#8095,#8096,#8097,#8098)) ;
#8276 = CLOSED_SHELL('',(#8099,#8100,#8101)) ;
#8277 = CLOSED_SHELL('',(#8102,#8103,#8104)) ;
#8278 = CLOSED_SHELL('',(#8105,#8106,#8107)) ;
#8279 = CLOSED_SHELL('',(#8108,#8109,#8110)) ;
#8280 = CLOSED_SHELL('',(#8111,#8112,#8113,#8114,#8115,#8116,#8117,#8118,
#8119,#8120,#8121,#8122,#8123,#8124,#8125,#8126,#8127,#8128,#8129,#8130,
#8131,#8132,#8133,#8134,#8135,#8136,#8137,#8138,#8139,#8140,#8141,#8142,
#8143,#8144,#8145,#8146,#8147,#8148,#8149,#8150,#8151,#8152,#8153,#8154,
#8155,#8156,#8157,#8158,#8159,#8160,#8161,#8162,#8163,#8164,#8165,#8166,
#8167,#8168,#8169,#8170,#8171,#8172,#8173,#8174,#8175)) ;
#8281 = CLOSED_SHELL('',(#8176,#8177,#8178,#8179,#8180,#8181,#8182,#8183,
#8184,#8185,#8186)) ;
#8282 = CLOSED_SHELL('',(#8187,#8188,#8189,#8190,#8191,#8192,#8193,#8194,
#8195,#8196,#8197,#8198)) ;
#8283 = CLOSED_SHELL('',(#8199,#8200,#8201,#8202)) ;
#8284 = CLOSED_SHELL('',(#8203,#8204,#8205)) ;
#8285 = CLOSED_SHELL('',(#8206,#8207,#8208)) ;
#8286 = CLOSED_SHELL('',(#8209,#8210,#8211)) ;
#8287 = CLOSED_SHELL('',(#8212,#8213,#8214)) ;
#8288 = CLOSED_SHELL('',(#8215,#8216,#8217)) ;
#8289 = CLOSED_SHELL('',(#8218,#8219,#8220,#8221,#8222,#8223,#8224,#8225,
#8226,#8227,#8228,#8229)) ;
#8290 = CLOSED_SHELL('',(#8230,#8231,#8232)) ;
#8291 = CLOSED_SHELL('',(#8233,#8234,#8235)) ;
#8292 = CLOSED_SHELL('',(#8236,#8237,#8238)) ;
#8293 = CLOSED_SHELL('',(#8239,#8240,#8241)) ;
#8294 = CLOSED_SHELL('',(#8242,#8243,#8244,#8245,#8246)) ;
#8295 = CLOSED_SHELL('',(#8247,#8248,#8249,#8250,#8251)) ;
#8296 = DERIVED_UNIT_ELEMENT(#8366,1.) ;
#8297 = DERIVED_UNIT_ELEMENT(#15486,-3.) ;
#8298 = DERIVED_UNIT_ELEMENT(#8366,1.) ;
#8299 = DERIVED_UNIT_ELEMENT(#15486,-3.) ;
#8300 = DERIVED_UNIT_ELEMENT(#8366,1.) ;
#8301 = DERIVED_UNIT_ELEMENT(#15486,-3.) ;
#8302 = DERIVED_UNIT_ELEMENT(#8366,1.) ;
#8303 = DERIVED_UNIT_ELEMENT(#15486,-3.) ;
#8304 = DERIVED_UNIT_ELEMENT(#8366,1.) ;
#8305 = DERIVED_UNIT_ELEMENT(#15486,-3.) ;
#8306 = DERIVED_UNIT_ELEMENT(#8366,1.) ;
#8307 = DERIVED_UNIT_ELEMENT(#15486,-3.) ;
#8308 = DERIVED_UNIT_ELEMENT(#8366,1.) ;
#8309 = DERIVED_UNIT_ELEMENT(#15486,-3.) ;
#8310 = DERIVED_UNIT_ELEMENT(#8366,1.) ;
#8311 = DERIVED_UNIT_ELEMENT(#15486,-3.) ;
#8312 = DERIVED_UNIT_ELEMENT(#8366,1.) ;
#8313 = DERIVED_UNIT_ELEMENT(#15486,-3.) ;
#8314 = DERIVED_UNIT_ELEMENT(#8366,1.) ;
#8315 = DERIVED_UNIT_ELEMENT(#15486,-3.) ;
#8316 = DERIVED_UNIT_ELEMENT(#8366,1.) ;
#8317 = DERIVED_UNIT_ELEMENT(#15486,-3.) ;
#8318 = DERIVED_UNIT_ELEMENT(#8366,1.) ;
#8319 = DERIVED_UNIT_ELEMENT(#15486,-3.) ;
#8320 = DERIVED_UNIT_ELEMENT(#8366,1.) ;
#8321 = DERIVED_UNIT_ELEMENT(#15486,-3.) ;
#8322 = DERIVED_UNIT_ELEMENT(#8366,1.) ;
#8323 = DERIVED_UNIT_ELEMENT(#15486,-3.) ;
#8324 = DERIVED_UNIT_ELEMENT(#8366,1.) ;
#8325 = DERIVED_UNIT_ELEMENT(#15486,-3.) ;
#8326 = DERIVED_UNIT_ELEMENT(#8366,1.) ;
#8327 = DERIVED_UNIT_ELEMENT(#15486,-3.) ;
#8328 = DERIVED_UNIT_ELEMENT(#8366,1.) ;
#8329 = DERIVED_UNIT_ELEMENT(#15486,-3.) ;
#8330 = DERIVED_UNIT_ELEMENT(#8366,1.) ;
#8331 = DERIVED_UNIT_ELEMENT(#15486,-3.) ;
#8332 = DERIVED_UNIT_ELEMENT(#8366,1.) ;
#8333 = DERIVED_UNIT_ELEMENT(#15486,-3.) ;
#8334 = DERIVED_UNIT_ELEMENT(#8366,1.) ;
#8335 = DERIVED_UNIT_ELEMENT(#15486,-3.) ;
#8336 = DERIVED_UNIT_ELEMENT(#8366,1.) ;
#8337 = DERIVED_UNIT_ELEMENT(#15486,-3.) ;
#8338 = DERIVED_UNIT_ELEMENT(#8366,1.) ;
#8339 = DERIVED_UNIT_ELEMENT(#15486,-3.) ;
#8340 = DERIVED_UNIT_ELEMENT(#8366,1.) ;
#8341 = DERIVED_UNIT_ELEMENT(#15486,-3.) ;
#8342 = DERIVED_UNIT_ELEMENT(#8366,1.) ;
#8343 = DERIVED_UNIT_ELEMENT(#15486,-3.) ;
#8344 = DERIVED_UNIT_ELEMENT(#8366,1.) ;
#8345 = DERIVED_UNIT_ELEMENT(#15486,-3.) ;
#8346 = DERIVED_UNIT_ELEMENT(#8366,1.) ;
#8347 = DERIVED_UNIT_ELEMENT(#15486,-3.) ;
#8348 = DERIVED_UNIT_ELEMENT(#8366,1.) ;
#8349 = DERIVED_UNIT_ELEMENT(#15486,-3.) ;
#8350 = DERIVED_UNIT_ELEMENT(#8366,1.) ;
#8351 = DERIVED_UNIT_ELEMENT(#15486,-3.) ;
#8352 = DERIVED_UNIT_ELEMENT(#8366,1.) ;
#8353 = DERIVED_UNIT_ELEMENT(#15486,-3.) ;
#8354 = DERIVED_UNIT_ELEMENT(#8366,1.) ;
#8355 = DERIVED_UNIT_ELEMENT(#15486,-3.) ;
#8356 = DERIVED_UNIT_ELEMENT(#8366,1.) ;
#8357 = DERIVED_UNIT_ELEMENT(#15486,-3.) ;
#8358 = DERIVED_UNIT_ELEMENT(#8366,1.) ;
#8359 = DERIVED_UNIT_ELEMENT(#15486,-3.) ;
#8360 = DERIVED_UNIT_ELEMENT(#8366,1.) ;
#8361 = DERIVED_UNIT_ELEMENT(#15486,-3.) ;
#8362 = DERIVED_UNIT_ELEMENT(#8366,1.) ;
#8363 = DERIVED_UNIT_ELEMENT(#15486,-3.) ;
#8364 = DERIVED_UNIT_ELEMENT(#8366,1.) ;
#8365 = DERIVED_UNIT_ELEMENT(#15486,-3.) ;
#8366 = (
MASS_UNIT()
NAMED_UNIT(*)
SI_UNIT(.KILO.,.GRAM.)
) ;
#8367 = DERIVED_UNIT((#8296,#8297)) ;
#8368 = DERIVED_UNIT((#8298,#8299)) ;
#8369 = DERIVED_UNIT((#8300,#8301)) ;
#8370 = DERIVED_UNIT((#8302,#8303)) ;
#8371 = DERIVED_UNIT((#8304,#8305)) ;
#8372 = DERIVED_UNIT((#8306,#8307)) ;
#8373 = DERIVED_UNIT((#8308,#8309)) ;
#8374 = DERIVED_UNIT((#8310,#8311)) ;
#8375 = DERIVED_UNIT((#8312,#8313)) ;
#8376 = DERIVED_UNIT((#8314,#8315)) ;
#8377 = DERIVED_UNIT((#8316,#8317)) ;
#8378 = DERIVED_UNIT((#8318,#8319)) ;
#8379 = DERIVED_UNIT((#8320,#8321)) ;
#8380 = DERIVED_UNIT((#8322,#8323)) ;
#8381 = DERIVED_UNIT((#8324,#8325)) ;
#8382 = DERIVED_UNIT((#8326,#8327)) ;
#8383 = DERIVED_UNIT((#8328,#8329)) ;
#8384 = DERIVED_UNIT((#8330,#8331)) ;
#8385 = DERIVED_UNIT((#8332,#8333)) ;
#8386 = DERIVED_UNIT((#8334,#8335)) ;
#8387 = DERIVED_UNIT((#8336,#8337)) ;
#8388 = DERIVED_UNIT((#8338,#8339)) ;
#8389 = DERIVED_UNIT((#8340,#8341)) ;
#8390 = DERIVED_UNIT((#8342,#8343)) ;
#8391 = DERIVED_UNIT((#8344,#8345)) ;
#8392 = DERIVED_UNIT((#8346,#8347)) ;
#8393 = DERIVED_UNIT((#8348,#8349)) ;
#8394 = DERIVED_UNIT((#8350,#8351)) ;
#8395 = DERIVED_UNIT((#8352,#8353)) ;
#8396 = DERIVED_UNIT((#8354,#8355)) ;
#8397 = DERIVED_UNIT((#8356,#8357)) ;
#8398 = DERIVED_UNIT((#8358,#8359)) ;
#8399 = DERIVED_UNIT((#8360,#8361)) ;
#8400 = DERIVED_UNIT((#8362,#8363)) ;
#8401 = DERIVED_UNIT((#8364,#8365)) ;
#8402 = MEASURE_REPRESENTATION_ITEM('density measure',
POSITIVE_RATIO_MEASURE(7850.),#8367) ;
#8403 = MEASURE_REPRESENTATION_ITEM('density measure',
POSITIVE_RATIO_MEASURE(7850.),#8368) ;
#8404 = MEASURE_REPRESENTATION_ITEM('density measure',
POSITIVE_RATIO_MEASURE(7850.),#8369) ;
#8405 = MEASURE_REPRESENTATION_ITEM('density measure',
POSITIVE_RATIO_MEASURE(7850.),#8370) ;
#8406 = MEASURE_REPRESENTATION_ITEM('density measure',
POSITIVE_RATIO_MEASURE(7850.),#8371) ;
#8407 = MEASURE_REPRESENTATION_ITEM('density measure',
POSITIVE_RATIO_MEASURE(7850.),#8372) ;
#8408 = MEASURE_REPRESENTATION_ITEM('density measure',
POSITIVE_RATIO_MEASURE(7850.),#8373) ;
#8409 = MEASURE_REPRESENTATION_ITEM('density measure',
POSITIVE_RATIO_MEASURE(7850.),#8374) ;
#8410 = MEASURE_REPRESENTATION_ITEM('density measure',
POSITIVE_RATIO_MEASURE(7850.),#8375) ;
#8411 = MEASURE_REPRESENTATION_ITEM('density measure',
POSITIVE_RATIO_MEASURE(7850.),#8376) ;
#8412 = MEASURE_REPRESENTATION_ITEM('density measure',
POSITIVE_RATIO_MEASURE(7850.),#8377) ;
#8413 = MEASURE_REPRESENTATION_ITEM('density measure',
POSITIVE_RATIO_MEASURE(7850.),#8378) ;
#8414 = MEASURE_REPRESENTATION_ITEM('density measure',
POSITIVE_RATIO_MEASURE(7850.),#8379) ;
#8415 = MEASURE_REPRESENTATION_ITEM('density measure',
POSITIVE_RATIO_MEASURE(7850.),#8380) ;
#8416 = MEASURE_REPRESENTATION_ITEM('density measure',
POSITIVE_RATIO_MEASURE(7850.),#8381) ;
#8417 = MEASURE_REPRESENTATION_ITEM('density measure',
POSITIVE_RATIO_MEASURE(7850.),#8382) ;
#8418 = MEASURE_REPRESENTATION_ITEM('density measure',
POSITIVE_RATIO_MEASURE(7850.),#8383) ;
#8419 = MEASURE_REPRESENTATION_ITEM('density measure',
POSITIVE_RATIO_MEASURE(7850.),#8384) ;
#8420 = MEASURE_REPRESENTATION_ITEM('density measure',
POSITIVE_RATIO_MEASURE(7850.),#8385) ;
#8421 = MEASURE_REPRESENTATION_ITEM('density measure',
POSITIVE_RATIO_MEASURE(7850.),#8386) ;
#8422 = MEASURE_REPRESENTATION_ITEM('density measure',
POSITIVE_RATIO_MEASURE(7850.),#8387) ;
#8423 = MEASURE_REPRESENTATION_ITEM('density measure',
POSITIVE_RATIO_MEASURE(7850.),#8388) ;
#8424 = MEASURE_REPRESENTATION_ITEM('density measure',
POSITIVE_RATIO_MEASURE(7850.),#8389) ;
#8425 = MEASURE_REPRESENTATION_ITEM('density measure',
POSITIVE_RATIO_MEASURE(7850.),#8390) ;
#8426 = MEASURE_REPRESENTATION_ITEM('density measure',
POSITIVE_RATIO_MEASURE(7850.),#8391) ;
#8427 = MEASURE_REPRESENTATION_ITEM('density measure',
POSITIVE_RATIO_MEASURE(7850.),#8392) ;
#8428 = MEASURE_REPRESENTATION_ITEM('density measure',
POSITIVE_RATIO_MEASURE(7850.),#8393) ;
#8429 = MEASURE_REPRESENTATION_ITEM('density measure',
POSITIVE_RATIO_MEASURE(7850.),#8394) ;
#8430 = MEASURE_REPRESENTATION_ITEM('density measure',
POSITIVE_RATIO_MEASURE(7850.),#8395) ;
#8431 = MEASURE_REPRESENTATION_ITEM('density measure',
POSITIVE_RATIO_MEASURE(7850.),#8396) ;
#8432 = MEASURE_REPRESENTATION_ITEM('density measure',
POSITIVE_RATIO_MEASURE(7850.),#8397) ;
#8433 = MEASURE_REPRESENTATION_ITEM('density measure',
POSITIVE_RATIO_MEASURE(7850.),#8398) ;
#8434 = MEASURE_REPRESENTATION_ITEM('density measure',
POSITIVE_RATIO_MEASURE(7850.),#8399) ;
#8435 = MEASURE_REPRESENTATION_ITEM('density measure',
POSITIVE_RATIO_MEASURE(7850.),#8400) ;
#8436 = MEASURE_REPRESENTATION_ITEM('density measure',
POSITIVE_RATIO_MEASURE(7850.),#8401) ;
#8437 = PROPERTY_DEFINITION_REPRESENTATION(#8612,#8507) ;
#8438 = PROPERTY_DEFINITION_REPRESENTATION(#8613,#8508) ;
#8439 = PROPERTY_DEFINITION_REPRESENTATION(#8614,#8509) ;
#8440 = PROPERTY_DEFINITION_REPRESENTATION(#8615,#8510) ;
#8441 = PROPERTY_DEFINITION_REPRESENTATION(#8616,#8511) ;
#8442 = PROPERTY_DEFINITION_REPRESENTATION(#8617,#8512) ;
#8443 = PROPERTY_DEFINITION_REPRESENTATION(#8618,#8513) ;
#8444 = PROPERTY_DEFINITION_REPRESENTATION(#8619,#8514) ;
#8445 = PROPERTY_DEFINITION_REPRESENTATION(#8620,#8515) ;
#8446 = PROPERTY_DEFINITION_REPRESENTATION(#8621,#8516) ;
#8447 = PROPERTY_DEFINITION_REPRESENTATION(#8622,#8517) ;
#8448 = PROPERTY_DEFINITION_REPRESENTATION(#8623,#8518) ;
#8449 = PROPERTY_DEFINITION_REPRESENTATION(#8624,#8519) ;
#8450 = PROPERTY_DEFINITION_REPRESENTATION(#8625,#8520) ;
#8451 = PROPERTY_DEFINITION_REPRESENTATION(#8626,#8521) ;
#8452 = PROPERTY_DEFINITION_REPRESENTATION(#8627,#8522) ;
#8453 = PROPERTY_DEFINITION_REPRESENTATION(#8628,#8523) ;
#8454 = PROPERTY_DEFINITION_REPRESENTATION(#8629,#8524) ;
#8455 = PROPERTY_DEFINITION_REPRESENTATION(#8630,#8525) ;
#8456 = PROPERTY_DEFINITION_REPRESENTATION(#8631,#8526) ;
#8457 = PROPERTY_DEFINITION_REPRESENTATION(#8632,#8527) ;
#8458 = PROPERTY_DEFINITION_REPRESENTATION(#8633,#8528) ;
#8459 = PROPERTY_DEFINITION_REPRESENTATION(#8634,#8529) ;
#8460 = PROPERTY_DEFINITION_REPRESENTATION(#8635,#8530) ;
#8461 = PROPERTY_DEFINITION_REPRESENTATION(#8636,#8531) ;
#8462 = PROPERTY_DEFINITION_REPRESENTATION(#8637,#8532) ;
#8463 = PROPERTY_DEFINITION_REPRESENTATION(#8638,#8533) ;
#8464 = PROPERTY_DEFINITION_REPRESENTATION(#8639,#8534) ;
#8465 = PROPERTY_DEFINITION_REPRESENTATION(#8640,#8535) ;
#8466 = PROPERTY_DEFINITION_REPRESENTATION(#8641,#8536) ;
#8467 = PROPERTY_DEFINITION_REPRESENTATION(#8642,#8537) ;
#8468 = PROPERTY_DEFINITION_REPRESENTATION(#8643,#8538) ;
#8469 = PROPERTY_DEFINITION_REPRESENTATION(#8644,#8539) ;
#8470 = PROPERTY_DEFINITION_REPRESENTATION(#8645,#8540) ;
#8471 = PROPERTY_DEFINITION_REPRESENTATION(#8646,#8541) ;
#8472 = PROPERTY_DEFINITION_REPRESENTATION(#8647,#8542) ;
#8473 = PROPERTY_DEFINITION_REPRESENTATION(#8648,#8543) ;
#8474 = PROPERTY_DEFINITION_REPRESENTATION(#8649,#8544) ;
#8475 = PROPERTY_DEFINITION_REPRESENTATION(#8650,#8545) ;
#8476 = PROPERTY_DEFINITION_REPRESENTATION(#8651,#8546) ;
#8477 = PROPERTY_DEFINITION_REPRESENTATION(#8652,#8547) ;
#8478 = PROPERTY_DEFINITION_REPRESENTATION(#8653,#8548) ;
#8479 = PROPERTY_DEFINITION_REPRESENTATION(#8654,#8549) ;
#8480 = PROPERTY_DEFINITION_REPRESENTATION(#8655,#8550) ;
#8481 = PROPERTY_DEFINITION_REPRESENTATION(#8656,#8551) ;
#8482 = PROPERTY_DEFINITION_REPRESENTATION(#8657,#8552) ;
#8483 = PROPERTY_DEFINITION_REPRESENTATION(#8658,#8553) ;
#8484 = PROPERTY_DEFINITION_REPRESENTATION(#8659,#8554) ;
#8485 = PROPERTY_DEFINITION_REPRESENTATION(#8660,#8555) ;
#8486 = PROPERTY_DEFINITION_REPRESENTATION(#8661,#8556) ;
#8487 = PROPERTY_DEFINITION_REPRESENTATION(#8662,#8557) ;
#8488 = PROPERTY_DEFINITION_REPRESENTATION(#8663,#8558) ;
#8489 = PROPERTY_DEFINITION_REPRESENTATION(#8664,#8559) ;
#8490 = PROPERTY_DEFINITION_REPRESENTATION(#8665,#8560) ;
#8491 = PROPERTY_DEFINITION_REPRESENTATION(#8666,#8561) ;
#8492 = PROPERTY_DEFINITION_REPRESENTATION(#8667,#8562) ;
#8493 = PROPERTY_DEFINITION_REPRESENTATION(#8668,#8563) ;
#8494 = PROPERTY_DEFINITION_REPRESENTATION(#8669,#8564) ;
#8495 = PROPERTY_DEFINITION_REPRESENTATION(#8670,#8565) ;
#8496 = PROPERTY_DEFINITION_REPRESENTATION(#8671,#8566) ;
#8497 = PROPERTY_DEFINITION_REPRESENTATION(#8672,#8567) ;
#8498 = PROPERTY_DEFINITION_REPRESENTATION(#8673,#8568) ;
#8499 = PROPERTY_DEFINITION_REPRESENTATION(#8674,#8569) ;
#8500 = PROPERTY_DEFINITION_REPRESENTATION(#8675,#8570) ;
#8501 = PROPERTY_DEFINITION_REPRESENTATION(#8676,#8571) ;
#8502 = PROPERTY_DEFINITION_REPRESENTATION(#8677,#8572) ;
#8503 = PROPERTY_DEFINITION_REPRESENTATION(#8678,#8573) ;
#8504 = PROPERTY_DEFINITION_REPRESENTATION(#8679,#8574) ;
#8505 = PROPERTY_DEFINITION_REPRESENTATION(#8680,#8575) ;
#8506 = PROPERTY_DEFINITION_REPRESENTATION(#8681,#8576) ;
#8507 = REPRESENTATION('material name',(#8577),#15444) ;
#8508 = REPRESENTATION('density',(#8402),#15444) ;
#8509 = REPRESENTATION('material name',(#8578),#15445) ;
#8510 = REPRESENTATION('density',(#8403),#15445) ;
#8511 = REPRESENTATION('material name',(#8579),#15447) ;
#8512 = REPRESENTATION('density',(#8404),#15447) ;
#8513 = REPRESENTATION('material name',(#8580),#15448) ;
#8514 = REPRESENTATION('density',(#8405),#15448) ;
#8515 = REPRESENTATION('material name',(#8581),#15449) ;
#8516 = REPRESENTATION('density',(#8406),#15449) ;
#8517 = REPRESENTATION('material name',(#8582),#15450) ;
#8518 = REPRESENTATION('density',(#8407),#15450) ;
#8519 = REPRESENTATION('material name',(#8583),#15452) ;
#8520 = REPRESENTATION('density',(#8408),#15452) ;
#8521 = REPRESENTATION('material name',(#8584),#15453) ;
#8522 = REPRESENTATION('density',(#8409),#15453) ;
#8523 = REPRESENTATION('material name',(#8585),#15454) ;
#8524 = REPRESENTATION('density',(#8410),#15454) ;
#8525 = REPRESENTATION('material name',(#8586),#15455) ;
#8526 = REPRESENTATION('density',(#8411),#15455) ;
#8527 = REPRESENTATION('material name',(#8587),#15456) ;
#8528 = REPRESENTATION('density',(#8412),#15456) ;
#8529 = REPRESENTATION('material name',(#8588),#15457) ;
#8530 = REPRESENTATION('density',(#8413),#15457) ;
#8531 = REPRESENTATION('material name',(#8589),#15458) ;
#8532 = REPRESENTATION('density',(#8414),#15458) ;
#8533 = REPRESENTATION('material name',(#8590),#15459) ;
#8534 = REPRESENTATION('density',(#8415),#15459) ;
#8535 = REPRESENTATION('material name',(#8591),#15460) ;
#8536 = REPRESENTATION('density',(#8416),#15460) ;
#8537 = REPRESENTATION('material name',(#8592),#15462) ;
#8538 = REPRESENTATION('density',(#8417),#15462) ;
#8539 = REPRESENTATION('material name',(#8593),#15463) ;
#8540 = REPRESENTATION('density',(#8418),#15463) ;
#8541 = REPRESENTATION('material name',(#8594),#15464) ;
#8542 = REPRESENTATION('density',(#8419),#15464) ;
#8543 = REPRESENTATION('material name',(#8595),#15465) ;
#8544 = REPRESENTATION('density',(#8420),#15465) ;
#8545 = REPRESENTATION('material name',(#8596),#15466) ;
#8546 = REPRESENTATION('density',(#8421),#15466) ;
#8547 = REPRESENTATION('material name',(#8597),#15467) ;
#8548 = REPRESENTATION('density',(#8422),#15467) ;
#8549 = REPRESENTATION('material name',(#8598),#15468) ;
#8550 = REPRESENTATION('density',(#8423),#15468) ;
#8551 = REPRESENTATION('material name',(#8599),#15469) ;
#8552 = REPRESENTATION('density',(#8424),#15469) ;
#8553 = REPRESENTATION('material name',(#8600),#15470) ;
#8554 = REPRESENTATION('density',(#8425),#15470) ;
#8555 = REPRESENTATION('material name',(#8601),#15471) ;
#8556 = REPRESENTATION('density',(#8426),#15471) ;
#8557 = REPRESENTATION('material name',(#8602),#15472) ;
#8558 = REPRESENTATION('density',(#8427),#15472) ;
#8559 = REPRESENTATION('material name',(#8603),#15474) ;
#8560 = REPRESENTATION('density',(#8428),#15474) ;
#8561 = REPRESENTATION('material name',(#8604),#15475) ;
#8562 = REPRESENTATION('density',(#8429),#15475) ;
#8563 = REPRESENTATION('material name',(#8605),#15476) ;
#8564 = REPRESENTATION('density',(#8430),#15476) ;
#8565 = REPRESENTATION('material name',(#8606),#15477) ;
#8566 = REPRESENTATION('density',(#8431),#15477) ;
#8567 = REPRESENTATION('material name',(#8607),#15478) ;
#8568 = REPRESENTATION('density',(#8432),#15478) ;
#8569 = REPRESENTATION('material name',(#8608),#15479) ;
#8570 = REPRESENTATION('density',(#8433),#15479) ;
#8571 = REPRESENTATION('material name',(#8609),#15480) ;
#8572 = REPRESENTATION('density',(#8434),#15480) ;
#8573 = REPRESENTATION('material name',(#8610),#15482) ;
#8574 = REPRESENTATION('density',(#8435),#15482) ;
#8575 = REPRESENTATION('material name',(#8611),#15483) ;
#8576 = REPRESENTATION('density',(#8436),#15483) ;
#8577 = DESCRIPTIVE_REPRESENTATION_ITEM('Steel','Steel') ;
#8578 = DESCRIPTIVE_REPRESENTATION_ITEM('Steel','Steel') ;
#8579 = DESCRIPTIVE_REPRESENTATION_ITEM('Steel','Steel') ;
#8580 = DESCRIPTIVE_REPRESENTATION_ITEM('Steel','Steel') ;
#8581 = DESCRIPTIVE_REPRESENTATION_ITEM('Steel','Steel') ;
#8582 = DESCRIPTIVE_REPRESENTATION_ITEM('Steel','Steel') ;
#8583 = DESCRIPTIVE_REPRESENTATION_ITEM('Steel','Steel') ;
#8584 = DESCRIPTIVE_REPRESENTATION_ITEM('Steel','Steel') ;
#8585 = DESCRIPTIVE_REPRESENTATION_ITEM('Steel','Steel') ;
#8586 = DESCRIPTIVE_REPRESENTATION_ITEM('Steel','Steel') ;
#8587 = DESCRIPTIVE_REPRESENTATION_ITEM('Steel','Steel') ;
#8588 = DESCRIPTIVE_REPRESENTATION_ITEM('Steel','Steel') ;
#8589 = DESCRIPTIVE_REPRESENTATION_ITEM('Steel','Steel') ;
#8590 = DESCRIPTIVE_REPRESENTATION_ITEM('Steel','Steel') ;
#8591 = DESCRIPTIVE_REPRESENTATION_ITEM('Steel','Steel') ;
#8592 = DESCRIPTIVE_REPRESENTATION_ITEM('Steel','Steel') ;
#8593 = DESCRIPTIVE_REPRESENTATION_ITEM('Steel','Steel') ;
#8594 = DESCRIPTIVE_REPRESENTATION_ITEM('Steel','Steel') ;
#8595 = DESCRIPTIVE_REPRESENTATION_ITEM('Steel','Steel') ;
#8596 = DESCRIPTIVE_REPRESENTATION_ITEM('Steel','Steel') ;
#8597 = DESCRIPTIVE_REPRESENTATION_ITEM('Steel','Steel') ;
#8598 = DESCRIPTIVE_REPRESENTATION_ITEM('Steel','Steel') ;
#8599 = DESCRIPTIVE_REPRESENTATION_ITEM('Steel','Steel') ;
#8600 = DESCRIPTIVE_REPRESENTATION_ITEM('Steel','Steel') ;
#8601 = DESCRIPTIVE_REPRESENTATION_ITEM('Steel','Steel') ;
#8602 = DESCRIPTIVE_REPRESENTATION_ITEM('Steel','Steel') ;
#8603 = DESCRIPTIVE_REPRESENTATION_ITEM('Steel','Steel') ;
#8604 = DESCRIPTIVE_REPRESENTATION_ITEM('Steel','Steel') ;
#8605 = DESCRIPTIVE_REPRESENTATION_ITEM('Steel','Steel') ;
#8606 = DESCRIPTIVE_REPRESENTATION_ITEM('Steel','Steel') ;
#8607 = DESCRIPTIVE_REPRESENTATION_ITEM('Steel','Steel') ;
#8608 = DESCRIPTIVE_REPRESENTATION_ITEM('Steel','Steel') ;
#8609 = DESCRIPTIVE_REPRESENTATION_ITEM('Steel','Steel') ;
#8610 = DESCRIPTIVE_REPRESENTATION_ITEM('Steel','Steel') ;
#8611 = DESCRIPTIVE_REPRESENTATION_ITEM('Steel','Steel') ;
#8612 = PROPERTY_DEFINITION('material property','material name',#15663) ;
#8613 = PROPERTY_DEFINITION('material property','density of part',#15663) ;
#8614 = PROPERTY_DEFINITION('material property','material name',#15664) ;
#8615 = PROPERTY_DEFINITION('material property','density of part',#15664) ;
#8616 = PROPERTY_DEFINITION('material property','material name',#15666) ;
#8617 = PROPERTY_DEFINITION('material property','density of part',#15666) ;
#8618 = PROPERTY_DEFINITION('material property','material name',#15667) ;
#8619 = PROPERTY_DEFINITION('material property','density of part',#15667) ;
#8620 = PROPERTY_DEFINITION('material property','material name',#15668) ;
#8621 = PROPERTY_DEFINITION('material property','density of part',#15668) ;
#8622 = PROPERTY_DEFINITION('material property','material name',#15669) ;
#8623 = PROPERTY_DEFINITION('material property','density of part',#15669) ;
#8624 = PROPERTY_DEFINITION('material property','material name',#15671) ;
#8625 = PROPERTY_DEFINITION('material property','density of part',#15671) ;
#8626 = PROPERTY_DEFINITION('material property','material name',#15672) ;
#8627 = PROPERTY_DEFINITION('material property','density of part',#15672) ;
#8628 = PROPERTY_DEFINITION('material property','material name',#15673) ;
#8629 = PROPERTY_DEFINITION('material property','density of part',#15673) ;
#8630 = PROPERTY_DEFINITION('material property','material name',#15674) ;
#8631 = PROPERTY_DEFINITION('material property','density of part',#15674) ;
#8632 = PROPERTY_DEFINITION('material property','material name',#15675) ;
#8633 = PROPERTY_DEFINITION('material property','density of part',#15675) ;
#8634 = PROPERTY_DEFINITION('material property','material name',#15676) ;
#8635 = PROPERTY_DEFINITION('material property','density of part',#15676) ;
#8636 = PROPERTY_DEFINITION('material property','material name',#15677) ;
#8637 = PROPERTY_DEFINITION('material property','density of part',#15677) ;
#8638 = PROPERTY_DEFINITION('material property','material name',#15678) ;
#8639 = PROPERTY_DEFINITION('material property','density of part',#15678) ;
#8640 = PROPERTY_DEFINITION('material property','material name',#15679) ;
#8641 = PROPERTY_DEFINITION('material property','density of part',#15679) ;
#8642 = PROPERTY_DEFINITION('material property','material name',#15681) ;
#8643 = PROPERTY_DEFINITION('material property','density of part',#15681) ;
#8644 = PROPERTY_DEFINITION('material property','material name',#15682) ;
#8645 = PROPERTY_DEFINITION('material property','density of part',#15682) ;
#8646 = PROPERTY_DEFINITION('material property','material name',#15683) ;
#8647 = PROPERTY_DEFINITION('material property','density of part',#15683) ;
#8648 = PROPERTY_DEFINITION('material property','material name',#15684) ;
#8649 = PROPERTY_DEFINITION('material property','density of part',#15684) ;
#8650 = PROPERTY_DEFINITION('material property','material name',#15685) ;
#8651 = PROPERTY_DEFINITION('material property','density of part',#15685) ;
#8652 = PROPERTY_DEFINITION('material property','material name',#15686) ;
#8653 = PROPERTY_DEFINITION('material property','density of part',#15686) ;
#8654 = PROPERTY_DEFINITION('material property','material name',#15687) ;
#8655 = PROPERTY_DEFINITION('material property','density of part',#15687) ;
#8656 = PROPERTY_DEFINITION('material property','material name',#15688) ;
#8657 = PROPERTY_DEFINITION('material property','density of part',#15688) ;
#8658 = PROPERTY_DEFINITION('material property','material name',#15689) ;
#8659 = PROPERTY_DEFINITION('material property','density of part',#15689) ;
#8660 = PROPERTY_DEFINITION('material property','material name',#15690) ;
#8661 = PROPERTY_DEFINITION('material property','density of part',#15690) ;
#8662 = PROPERTY_DEFINITION('material property','material name',#15691) ;
#8663 = PROPERTY_DEFINITION('material property','density of part',#15691) ;
#8664 = PROPERTY_DEFINITION('material property','material name',#15693) ;
#8665 = PROPERTY_DEFINITION('material property','density of part',#15693) ;
#8666 = PROPERTY_DEFINITION('material property','material name',#15694) ;
#8667 = PROPERTY_DEFINITION('material property','density of part',#15694) ;
#8668 = PROPERTY_DEFINITION('material property','material name',#15695) ;
#8669 = PROPERTY_DEFINITION('material property','density of part',#15695) ;
#8670 = PROPERTY_DEFINITION('material property','material name',#15696) ;
#8671 = PROPERTY_DEFINITION('material property','density of part',#15696) ;
#8672 = PROPERTY_DEFINITION('material property','material name',#15697) ;
#8673 = PROPERTY_DEFINITION('material property','density of part',#15697) ;
#8674 = PROPERTY_DEFINITION('material property','material name',#15698) ;
#8675 = PROPERTY_DEFINITION('material property','density of part',#15698) ;
#8676 = PROPERTY_DEFINITION('material property','material name',#15699) ;
#8677 = PROPERTY_DEFINITION('material property','density of part',#15699) ;
#8678 = PROPERTY_DEFINITION('material property','material name',#15701) ;
#8679 = PROPERTY_DEFINITION('material property','density of part',#15701) ;
#8680 = PROPERTY_DEFINITION('material property','material name',#15702) ;
#8681 = PROPERTY_DEFINITION('material property','density of part',#15702) ;
#8682 = AXIS2_PLACEMENT_3D('',#12885,#9925,#9926) ;
#8683 = AXIS2_PLACEMENT_3D('',#12886,#9927,#9928) ;
#8684 = AXIS2_PLACEMENT_3D('',#12887,#9929,#9930) ;
#8685 = AXIS2_PLACEMENT_3D('',#12888,#9931,#9932) ;
#8686 = AXIS2_PLACEMENT_3D('',#12897,#9937,#9938) ;
#8687 = AXIS2_PLACEMENT_3D('',#12907,#9944,#9945) ;
#8688 = AXIS2_PLACEMENT_3D('',#12915,#9950,#9951) ;
#8689 = AXIS2_PLACEMENT_3D('',#12919,#9954,#9955) ;
#8690 = AXIS2_PLACEMENT_3D('',#12921,#9957,#9958) ;
#8691 = AXIS2_PLACEMENT_3D('',#12926,#9961,#9962) ;
#8692 = AXIS2_PLACEMENT_3D('',#12928,#9963,#9964) ;
#8693 = AXIS2_PLACEMENT_3D('',#12946,#9973,#9974) ;
#8694 = AXIS2_PLACEMENT_3D('',#12948,#9975,#9976) ;
#8695 = AXIS2_PLACEMENT_3D('',#12949,#9977,#9978) ;
#8696 = AXIS2_PLACEMENT_3D('',#12951,#9979,#9980) ;
#8697 = AXIS2_PLACEMENT_3D('',#12954,#9982,#9983) ;
#8698 = AXIS2_PLACEMENT_3D('',#12955,#9984,#9985) ;
#8699 = AXIS2_PLACEMENT_3D('',#12956,#9986,#9987) ;
#8700 = AXIS2_PLACEMENT_3D('',#12958,#9988,#9989) ;
#8701 = AXIS2_PLACEMENT_3D('',#12961,#9991,#9992) ;
#8702 = AXIS2_PLACEMENT_3D('',#12962,#9993,#9994) ;
#8703 = AXIS2_PLACEMENT_3D('',#12963,#9995,#9996) ;
#8704 = AXIS2_PLACEMENT_3D('',#12965,#9997,#9998) ;
#8705 = AXIS2_PLACEMENT_3D('',#12968,#10000,#10001) ;
#8706 = AXIS2_PLACEMENT_3D('',#12969,#10002,#10003) ;
#8707 = AXIS2_PLACEMENT_3D('',#12978,#10008,#10009) ;
#8708 = AXIS2_PLACEMENT_3D('',#12984,#10013,#10014) ;
#8709 = AXIS2_PLACEMENT_3D('',#12988,#10017,#10018) ;
#8710 = AXIS2_PLACEMENT_3D('',#12992,#10021,#10022) ;
#8711 = AXIS2_PLACEMENT_3D('',#13002,#10028,#10029) ;
#8712 = AXIS2_PLACEMENT_3D('',#13004,#10030,#10031) ;
#8713 = AXIS2_PLACEMENT_3D('',#13007,#10033,#10034) ;
#8714 = AXIS2_PLACEMENT_3D('',#13008,#10035,#10036) ;
#8715 = AXIS2_PLACEMENT_3D('',#13017,#10041,#10042) ;
#8716 = AXIS2_PLACEMENT_3D('',#13023,#10046,#10047) ;
#8717 = AXIS2_PLACEMENT_3D('',#13027,#10050,#10051) ;
#8718 = AXIS2_PLACEMENT_3D('',#13031,#10054,#10055) ;
#8719 = AXIS2_PLACEMENT_3D('',#13041,#10061,#10062) ;
#8720 = AXIS2_PLACEMENT_3D('',#13043,#10063,#10064) ;
#8721 = AXIS2_PLACEMENT_3D('',#13046,#10066,#10067) ;
#8722 = AXIS2_PLACEMENT_3D('',#13047,#10068,#10069) ;
#8723 = AXIS2_PLACEMENT_3D('',#13049,#10070,#10071) ;
#8724 = AXIS2_PLACEMENT_3D('',#13051,#10073,#10074) ;
#8725 = AXIS2_PLACEMENT_3D('',#13052,#10075,#10076) ;
#8726 = AXIS2_PLACEMENT_3D('',#13053,#10077,#10078) ;
#8727 = AXIS2_PLACEMENT_3D('',#13055,#10079,#10080) ;
#8728 = AXIS2_PLACEMENT_3D('',#13058,#10082,#10083) ;
#8729 = AXIS2_PLACEMENT_3D('',#13059,#10084,#10085) ;
#8730 = AXIS2_PLACEMENT_3D('',#13061,#10086,#10087) ;
#8731 = AXIS2_PLACEMENT_3D('',#13063,#10089,#10090) ;
#8732 = AXIS2_PLACEMENT_3D('',#13064,#10091,#10092) ;
#8733 = AXIS2_PLACEMENT_3D('',#13066,#10093,#10094) ;
#8734 = AXIS2_PLACEMENT_3D('',#13069,#10096,#10097) ;
#8735 = AXIS2_PLACEMENT_3D('',#13070,#10098,#10099) ;
#8736 = AXIS2_PLACEMENT_3D('',#13072,#10100,#10101) ;
#8737 = AXIS2_PLACEMENT_3D('',#13074,#10103,#10104) ;
#8738 = AXIS2_PLACEMENT_3D('',#13075,#10105,#10106) ;
#8739 = AXIS2_PLACEMENT_3D('',#13076,#10107,#10108) ;
#8740 = AXIS2_PLACEMENT_3D('',#13078,#10109,#10110) ;
#8741 = AXIS2_PLACEMENT_3D('',#13081,#10112,#10113) ;
#8742 = AXIS2_PLACEMENT_3D('',#13082,#10114,#10115) ;
#8743 = AXIS2_PLACEMENT_3D('',#13084,#10116,#10117) ;
#8744 = AXIS2_PLACEMENT_3D('',#13087,#10119,#10120) ;
#8745 = AXIS2_PLACEMENT_3D('',#13088,#10121,#10122) ;
#8746 = AXIS2_PLACEMENT_3D('',#13097,#10127,#10128) ;
#8747 = AXIS2_PLACEMENT_3D('',#13100,#10131,#10132) ;
#8748 = AXIS2_PLACEMENT_3D('',#13102,#10134,#10135) ;
#8749 = AXIS2_PLACEMENT_3D('',#13104,#10137,#10138) ;
#8750 = AXIS2_PLACEMENT_3D('',#13105,#10139,#10140) ;
#8751 = AXIS2_PLACEMENT_3D('',#13114,#10145,#10146) ;
#8752 = AXIS2_PLACEMENT_3D('',#13117,#10149,#10150) ;
#8753 = AXIS2_PLACEMENT_3D('',#13119,#10152,#10153) ;
#8754 = AXIS2_PLACEMENT_3D('',#13121,#10155,#10156) ;
#8755 = AXIS2_PLACEMENT_3D('',#13122,#10157,#10158) ;
#8756 = AXIS2_PLACEMENT_3D('',#13124,#10159,#10160) ;
#8757 = AXIS2_PLACEMENT_3D('',#13126,#10162,#10163) ;
#8758 = AXIS2_PLACEMENT_3D('',#13130,#10166,#10167) ;
#8759 = AXIS2_PLACEMENT_3D('',#13132,#10169,#10170) ;
#8760 = AXIS2_PLACEMENT_3D('',#13133,#10171,#10172) ;
#8761 = AXIS2_PLACEMENT_3D('',#13136,#10175,#10176) ;
#8762 = AXIS2_PLACEMENT_3D('',#13139,#10179,#10180) ;
#8763 = AXIS2_PLACEMENT_3D('',#13140,#10181,#10182) ;
#8764 = AXIS2_PLACEMENT_3D('',#13141,#10183,#10184) ;
#8765 = AXIS2_PLACEMENT_3D('',#13142,#10185,#10186) ;
#8766 = AXIS2_PLACEMENT_3D('',#13147,#10188,#10189) ;
#8767 = AXIS2_PLACEMENT_3D('',#13150,#10191,#10192) ;
#8768 = AXIS2_PLACEMENT_3D('',#13151,#10193,#10194) ;
#8769 = AXIS2_PLACEMENT_3D('',#13155,#10196,#10197) ;
#8770 = AXIS2_PLACEMENT_3D('',#13158,#10199,#10200) ;
#8771 = AXIS2_PLACEMENT_3D('',#13159,#10201,#10202) ;
#8772 = AXIS2_PLACEMENT_3D('',#13163,#10204,#10205) ;
#8773 = AXIS2_PLACEMENT_3D('',#13165,#10207,#10208) ;
#8774 = AXIS2_PLACEMENT_3D('',#13176,#10214,#10215) ;
#8775 = AXIS2_PLACEMENT_3D('',#13177,#10216,#10217) ;
#8776 = AXIS2_PLACEMENT_3D('',#13179,#10219,#10220) ;
#8777 = AXIS2_PLACEMENT_3D('',#13182,#10222,#10223) ;
#8778 = AXIS2_PLACEMENT_3D('',#13183,#10224,#10225) ;
#8779 = AXIS2_PLACEMENT_3D('',#13188,#10227,#10228) ;
#8780 = AXIS2_PLACEMENT_3D('',#13191,#10230,#10231) ;
#8781 = AXIS2_PLACEMENT_3D('',#13192,#10232,#10233) ;
#8782 = AXIS2_PLACEMENT_3D('',#13197,#10235,#10236) ;
#8783 = AXIS2_PLACEMENT_3D('',#13200,#10238,#10239) ;
#8784 = AXIS2_PLACEMENT_3D('',#13201,#10240,#10241) ;
#8785 = AXIS2_PLACEMENT_3D('',#13205,#10244,#10245) ;
#8786 = AXIS2_PLACEMENT_3D('',#13206,#10246,#10247) ;
#8787 = AXIS2_PLACEMENT_3D('',#13213,#10252,#10253) ;
#8788 = AXIS2_PLACEMENT_3D('',#13215,#10255,#10256) ;
#8789 = AXIS2_PLACEMENT_3D('',#13219,#10259,#10260) ;
#8790 = AXIS2_PLACEMENT_3D('',#13222,#10262,#10263) ;
#8791 = AXIS2_PLACEMENT_3D('',#13223,#10264,#10265) ;
#8792 = AXIS2_PLACEMENT_3D('',#13225,#10266,#10267) ;
#8793 = AXIS2_PLACEMENT_3D('',#13227,#10269,#10270) ;
#8794 = AXIS2_PLACEMENT_3D('',#13231,#10273,#10274) ;
#8795 = AXIS2_PLACEMENT_3D('',#13233,#10276,#10277) ;
#8796 = AXIS2_PLACEMENT_3D('',#13234,#10278,#10279) ;
#8797 = AXIS2_PLACEMENT_3D('',#13235,#10280,#10281) ;
#8798 = AXIS2_PLACEMENT_3D('',#13236,#10282,#10283) ;
#8799 = AXIS2_PLACEMENT_3D('',#13237,#10284,#10285) ;
#8800 = AXIS2_PLACEMENT_3D('',#13238,#10286,#10287) ;
#8801 = AXIS2_PLACEMENT_3D('',#13240,#10288,#10289) ;
#8802 = AXIS2_PLACEMENT_3D('',#13243,#10291,#10292) ;
#8803 = AXIS2_PLACEMENT_3D('',#13244,#10293,#10294) ;
#8804 = AXIS2_PLACEMENT_3D('',#13245,#10295,#10296) ;
#8805 = AXIS2_PLACEMENT_3D('',#13254,#10301,#10302) ;
#8806 = AXIS2_PLACEMENT_3D('',#13260,#10306,#10307) ;
#8807 = AXIS2_PLACEMENT_3D('',#13264,#10310,#10311) ;
#8808 = AXIS2_PLACEMENT_3D('',#13268,#10314,#10315) ;
#8809 = AXIS2_PLACEMENT_3D('',#13270,#10317,#10318) ;
#8810 = AXIS2_PLACEMENT_3D('',#13279,#10323,#10324) ;
#8811 = AXIS2_PLACEMENT_3D('',#13285,#10328,#10329) ;
#8812 = AXIS2_PLACEMENT_3D('',#13289,#10332,#10333) ;
#8813 = AXIS2_PLACEMENT_3D('',#13293,#10336,#10337) ;
#8814 = AXIS2_PLACEMENT_3D('',#13295,#10339,#10340) ;
#8815 = AXIS2_PLACEMENT_3D('',#13304,#10345,#10346) ;
#8816 = AXIS2_PLACEMENT_3D('',#13310,#10350,#10351) ;
#8817 = AXIS2_PLACEMENT_3D('',#13314,#10354,#10355) ;
#8818 = AXIS2_PLACEMENT_3D('',#13318,#10358,#10359) ;
#8819 = AXIS2_PLACEMENT_3D('',#13320,#10361,#10362) ;
#8820 = AXIS2_PLACEMENT_3D('',#13322,#10363,#10364) ;
#8821 = AXIS2_PLACEMENT_3D('',#13325,#10366,#10367) ;
#8822 = AXIS2_PLACEMENT_3D('',#13326,#10368,#10369) ;
#8823 = AXIS2_PLACEMENT_3D('',#13328,#10370,#10371) ;
#8824 = AXIS2_PLACEMENT_3D('',#13331,#10373,#10374) ;
#8825 = AXIS2_PLACEMENT_3D('',#13332,#10375,#10376) ;
#8826 = AXIS2_PLACEMENT_3D('',#13333,#10377,#10378) ;
#8827 = AXIS2_PLACEMENT_3D('',#13335,#10379,#10380) ;
#8828 = AXIS2_PLACEMENT_3D('',#13336,#10381,#10382) ;
#8829 = AXIS2_PLACEMENT_3D('',#13338,#10383,#10384) ;
#8830 = AXIS2_PLACEMENT_3D('',#13340,#10386,#10387) ;
#8831 = AXIS2_PLACEMENT_3D('',#13342,#10388,#10389) ;
#8832 = AXIS2_PLACEMENT_3D('',#13345,#10391,#10392) ;
#8833 = AXIS2_PLACEMENT_3D('',#13346,#10393,#10394) ;
#8834 = AXIS2_PLACEMENT_3D('',#13347,#10395,#10396) ;
#8835 = AXIS2_PLACEMENT_3D('',#13349,#10397,#10398) ;
#8836 = AXIS2_PLACEMENT_3D('',#13350,#10399,#10400) ;
#8837 = AXIS2_PLACEMENT_3D('',#13352,#10401,#10402) ;
#8838 = AXIS2_PLACEMENT_3D('',#13354,#10404,#10405) ;
#8839 = AXIS2_PLACEMENT_3D('',#13355,#10406,#10407) ;
#8840 = AXIS2_PLACEMENT_3D('',#13356,#10408,#10409) ;
#8841 = AXIS2_PLACEMENT_3D('',#13357,#10410,#10411) ;
#8842 = AXIS2_PLACEMENT_3D('',#13359,#10412,#10413) ;
#8843 = AXIS2_PLACEMENT_3D('',#13362,#10415,#10416) ;
#8844 = AXIS2_PLACEMENT_3D('',#13363,#10417,#10418) ;
#8845 = AXIS2_PLACEMENT_3D('',#13365,#10419,#10420) ;
#8846 = AXIS2_PLACEMENT_3D('',#13368,#10422,#10423) ;
#8847 = AXIS2_PLACEMENT_3D('',#13369,#10424,#10425) ;
#8848 = AXIS2_PLACEMENT_3D('',#13370,#10426,#10427) ;
#8849 = AXIS2_PLACEMENT_3D('',#13371,#10428,#10429) ;
#8850 = AXIS2_PLACEMENT_3D('',#13372,#10430,#10431) ;
#8851 = AXIS2_PLACEMENT_3D('',#13374,#10432,#10433) ;
#8852 = AXIS2_PLACEMENT_3D('',#13377,#10435,#10436) ;
#8853 = AXIS2_PLACEMENT_3D('',#13378,#10437,#10438) ;
#8854 = AXIS2_PLACEMENT_3D('',#13380,#10439,#10440) ;
#8855 = AXIS2_PLACEMENT_3D('',#13383,#10442,#10443) ;
#8856 = AXIS2_PLACEMENT_3D('',#13384,#10444,#10445) ;
#8857 = AXIS2_PLACEMENT_3D('',#13385,#10446,#10447) ;
#8858 = AXIS2_PLACEMENT_3D('',#13386,#10448,#10449) ;
#8859 = AXIS2_PLACEMENT_3D('',#13387,#10450,#10451) ;
#8860 = AXIS2_PLACEMENT_3D('',#13389,#10452,#10453) ;
#8861 = AXIS2_PLACEMENT_3D('',#13391,#10454,#10455) ;
#8862 = AXIS2_PLACEMENT_3D('',#13392,#10456,#10457) ;
#8863 = AXIS2_PLACEMENT_3D('',#13394,#10458,#10459) ;
#8864 = AXIS2_PLACEMENT_3D('',#13396,#10461,#10462) ;
#8865 = AXIS2_PLACEMENT_3D('',#13397,#10463,#10464) ;
#8866 = AXIS2_PLACEMENT_3D('',#13398,#10465,#10466) ;
#8867 = AXIS2_PLACEMENT_3D('',#13399,#10467,#10468) ;
#8868 = AXIS2_PLACEMENT_3D('',#13400,#10469,#10470) ;
#8869 = AXIS2_PLACEMENT_3D('',#13401,#10471,#10472) ;
#8870 = AXIS2_PLACEMENT_3D('',#13402,#10473,#10474) ;
#8871 = AXIS2_PLACEMENT_3D('',#13403,#10475,#10476) ;
#8872 = AXIS2_PLACEMENT_3D('',#13405,#10477,#10478) ;
#8873 = AXIS2_PLACEMENT_3D('',#13408,#10480,#10481) ;
#8874 = AXIS2_PLACEMENT_3D('',#13409,#10482,#10483) ;
#8875 = AXIS2_PLACEMENT_3D('',#13411,#10484,#10485) ;
#8876 = AXIS2_PLACEMENT_3D('',#13414,#10487,#10488) ;
#8877 = AXIS2_PLACEMENT_3D('',#13415,#10489,#10490) ;
#8878 = AXIS2_PLACEMENT_3D('',#13417,#10491,#10492) ;
#8879 = AXIS2_PLACEMENT_3D('',#13418,#10493,#10494) ;
#8880 = AXIS2_PLACEMENT_3D('',#13421,#10496,#10497) ;
#8881 = AXIS2_PLACEMENT_3D('',#13422,#10498,#10499) ;
#8882 = AXIS2_PLACEMENT_3D('',#13423,#10500,#10501) ;
#8883 = AXIS2_PLACEMENT_3D('',#13424,#10502,#10503) ;
#8884 = AXIS2_PLACEMENT_3D('',#13425,#10504,#10505) ;
#8885 = AXIS2_PLACEMENT_3D('',#13427,#10506,#10507) ;
#8886 = AXIS2_PLACEMENT_3D('',#13430,#10509,#10510) ;
#8887 = AXIS2_PLACEMENT_3D('',#13431,#10511,#10512) ;
#8888 = AXIS2_PLACEMENT_3D('',#13432,#10513,#10514) ;
#8889 = AXIS2_PLACEMENT_3D('',#13434,#10515,#10516) ;
#8890 = AXIS2_PLACEMENT_3D('',#13437,#10518,#10519) ;
#8891 = AXIS2_PLACEMENT_3D('',#13438,#10520,#10521) ;
#8892 = AXIS2_PLACEMENT_3D('',#13439,#10522,#10523) ;
#8893 = AXIS2_PLACEMENT_3D('',#13440,#10524,#10525) ;
#8894 = AXIS2_PLACEMENT_3D('',#13441,#10526,#10527) ;
#8895 = AXIS2_PLACEMENT_3D('',#13443,#10528,#10529) ;
#8896 = AXIS2_PLACEMENT_3D('',#13446,#10531,#10532) ;
#8897 = AXIS2_PLACEMENT_3D('',#13447,#10533,#10534) ;
#8898 = AXIS2_PLACEMENT_3D('',#13448,#10535,#10536) ;
#8899 = AXIS2_PLACEMENT_3D('',#13449,#10537,#10538) ;
#8900 = AXIS2_PLACEMENT_3D('',#13450,#10539,#10540) ;
#8901 = AXIS2_PLACEMENT_3D('',#13459,#10545,#10546) ;
#8902 = AXIS2_PLACEMENT_3D('',#13462,#10547,#10548) ;
#8903 = AXIS2_PLACEMENT_3D('',#13466,#10551,#10552) ;
#8904 = AXIS2_PLACEMENT_3D('',#13472,#10556,#10557) ;
#8905 = AXIS2_PLACEMENT_3D('',#13474,#10558,#10559) ;
#8906 = AXIS2_PLACEMENT_3D('',#13476,#10561,#10562) ;
#8907 = AXIS2_PLACEMENT_3D('',#13478,#10563,#10564) ;
#8908 = AXIS2_PLACEMENT_3D('',#13480,#10566,#10567) ;
#8909 = AXIS2_PLACEMENT_3D('',#13482,#10568,#10569) ;
#8910 = AXIS2_PLACEMENT_3D('',#13484,#10571,#10572) ;
#8911 = AXIS2_PLACEMENT_3D('',#13486,#10574,#10575) ;
#8912 = AXIS2_PLACEMENT_3D('',#13488,#10577,#10578) ;
#8913 = AXIS2_PLACEMENT_3D('',#13490,#10579,#10580) ;
#8914 = AXIS2_PLACEMENT_3D('',#13493,#10582,#10583) ;
#8915 = AXIS2_PLACEMENT_3D('',#13494,#10584,#10585) ;
#8916 = AXIS2_PLACEMENT_3D('',#13497,#10586,#10587) ;
#8917 = AXIS2_PLACEMENT_3D('',#13498,#10588,#10589) ;
#8918 = AXIS2_PLACEMENT_3D('',#13499,#10590,#10591) ;
#8919 = AXIS2_PLACEMENT_3D('',#13503,#10593,#10594) ;
#8920 = AXIS2_PLACEMENT_3D('',#13506,#10596,#10597) ;
#8921 = AXIS2_PLACEMENT_3D('',#13508,#10598,#10599) ;
#8922 = AXIS2_PLACEMENT_3D('',#13510,#10601,#10602) ;
#8923 = AXIS2_PLACEMENT_3D('',#13512,#10603,#10604) ;
#8924 = AXIS2_PLACEMENT_3D('',#13515,#10606,#10607) ;
#8925 = AXIS2_PLACEMENT_3D('',#13516,#10608,#10609) ;
#8926 = AXIS2_PLACEMENT_3D('',#13517,#10610,#10611) ;
#8927 = AXIS2_PLACEMENT_3D('',#13518,#10612,#10613) ;
#8928 = AXIS2_PLACEMENT_3D('',#13520,#10614,#10615) ;
#8929 = AXIS2_PLACEMENT_3D('',#13521,#10616,#10617) ;
#8930 = AXIS2_PLACEMENT_3D('',#13524,#10619,#10620) ;
#8931 = AXIS2_PLACEMENT_3D('',#13525,#10621,#10622) ;
#8932 = AXIS2_PLACEMENT_3D('',#13526,#10623,#10624) ;
#8933 = AXIS2_PLACEMENT_3D('',#13527,#10625,#10626) ;
#8934 = AXIS2_PLACEMENT_3D('',#13530,#10627,#10628) ;
#8935 = AXIS2_PLACEMENT_3D('',#13531,#10629,#10630) ;
#8936 = AXIS2_PLACEMENT_3D('',#13534,#10631,#10632) ;
#8937 = AXIS2_PLACEMENT_3D('',#13535,#10633,#10634) ;
#8938 = AXIS2_PLACEMENT_3D('',#13536,#10635,#10636) ;
#8939 = AXIS2_PLACEMENT_3D('',#13537,#10637,#10638) ;
#8940 = AXIS2_PLACEMENT_3D('',#13538,#10639,#10640) ;
#8941 = AXIS2_PLACEMENT_3D('',#13539,#10641,#10642) ;
#8942 = AXIS2_PLACEMENT_3D('',#13541,#10643,#10644) ;
#8943 = AXIS2_PLACEMENT_3D('',#13543,#10645,#10646) ;
#8944 = AXIS2_PLACEMENT_3D('',#13544,#10647,#10648) ;
#8945 = AXIS2_PLACEMENT_3D('',#13569,#10649,#10650) ;
#8946 = AXIS2_PLACEMENT_3D('',#13570,#10651,#10652) ;
#8947 = AXIS2_PLACEMENT_3D('',#13573,#10653,#10654) ;
#8948 = AXIS2_PLACEMENT_3D('',#13575,#10655,#10656) ;
#8949 = AXIS2_PLACEMENT_3D('',#13577,#10658,#10659) ;
#8950 = AXIS2_PLACEMENT_3D('',#13578,#10660,#10661) ;
#8951 = AXIS2_PLACEMENT_3D('',#13580,#10662,#10663) ;
#8952 = AXIS2_PLACEMENT_3D('',#13582,#10664,#10665) ;
#8953 = AXIS2_PLACEMENT_3D('',#13583,#10666,#10667) ;
#8954 = AXIS2_PLACEMENT_3D('',#13608,#10668,#10669) ;
#8955 = AXIS2_PLACEMENT_3D('',#13609,#10670,#10671) ;
#8956 = AXIS2_PLACEMENT_3D('',#13612,#10673,#10674) ;
#8957 = AXIS2_PLACEMENT_3D('',#13613,#10675,#10676) ;
#8958 = AXIS2_PLACEMENT_3D('',#13614,#10677,#10678) ;
#8959 = AXIS2_PLACEMENT_3D('',#13616,#10679,#10680) ;
#8960 = AXIS2_PLACEMENT_3D('',#13618,#10682,#10683) ;
#8961 = AXIS2_PLACEMENT_3D('',#13619,#10684,#10685) ;
#8962 = AXIS2_PLACEMENT_3D('',#13622,#10687,#10688) ;
#8963 = AXIS2_PLACEMENT_3D('',#13623,#10689,#10690) ;
#8964 = AXIS2_PLACEMENT_3D('',#13624,#10691,#10692) ;
#8965 = AXIS2_PLACEMENT_3D('',#13625,#10693,#10694) ;
#8966 = AXIS2_PLACEMENT_3D('',#13626,#10695,#10696) ;
#8967 = AXIS2_PLACEMENT_3D('',#13627,#10697,#10698) ;
#8968 = AXIS2_PLACEMENT_3D('',#13628,#10699,#10700) ;
#8969 = AXIS2_PLACEMENT_3D('',#13630,#10701,#10702) ;
#8970 = AXIS2_PLACEMENT_3D('',#13633,#10704,#10705) ;
#8971 = AXIS2_PLACEMENT_3D('',#13634,#10706,#10707) ;
#8972 = AXIS2_PLACEMENT_3D('',#13636,#10708,#10709) ;
#8973 = AXIS2_PLACEMENT_3D('',#13639,#10711,#10712) ;
#8974 = AXIS2_PLACEMENT_3D('',#13640,#10713,#10714) ;
#8975 = AXIS2_PLACEMENT_3D('',#13641,#10715,#10716) ;
#8976 = AXIS2_PLACEMENT_3D('',#13642,#10717,#10718) ;
#8977 = AXIS2_PLACEMENT_3D('',#13643,#10719,#10720) ;
#8978 = AXIS2_PLACEMENT_3D('',#13645,#10721,#10722) ;
#8979 = AXIS2_PLACEMENT_3D('',#13648,#10724,#10725) ;
#8980 = AXIS2_PLACEMENT_3D('',#13649,#10726,#10727) ;
#8981 = AXIS2_PLACEMENT_3D('',#13651,#10728,#10729) ;
#8982 = AXIS2_PLACEMENT_3D('',#13654,#10731,#10732) ;
#8983 = AXIS2_PLACEMENT_3D('',#13655,#10733,#10734) ;
#8984 = AXIS2_PLACEMENT_3D('',#13657,#10735,#10736) ;
#8985 = AXIS2_PLACEMENT_3D('',#13658,#10737,#10738) ;
#8986 = AXIS2_PLACEMENT_3D('',#13661,#10740,#10741) ;
#8987 = AXIS2_PLACEMENT_3D('',#13662,#10742,#10743) ;
#8988 = AXIS2_PLACEMENT_3D('',#13663,#10744,#10745) ;
#8989 = AXIS2_PLACEMENT_3D('',#13664,#10746,#10747) ;
#8990 = AXIS2_PLACEMENT_3D('',#13665,#10748,#10749) ;
#8991 = AXIS2_PLACEMENT_3D('',#13667,#10750,#10751) ;
#8992 = AXIS2_PLACEMENT_3D('',#13670,#10753,#10754) ;
#8993 = AXIS2_PLACEMENT_3D('',#13671,#10755,#10756) ;
#8994 = AXIS2_PLACEMENT_3D('',#13672,#10757,#10758) ;
#8995 = AXIS2_PLACEMENT_3D('',#13673,#10759,#10760) ;
#8996 = AXIS2_PLACEMENT_3D('',#13674,#10761,#10762) ;
#8997 = AXIS2_PLACEMENT_3D('',#13676,#10763,#10764) ;
#8998 = AXIS2_PLACEMENT_3D('',#13679,#10766,#10767) ;
#8999 = AXIS2_PLACEMENT_3D('',#13680,#10768,#10769) ;
#9000 = AXIS2_PLACEMENT_3D('',#13681,#10770,#10771) ;
#9001 = AXIS2_PLACEMENT_3D('',#13682,#10772,#10773) ;
#9002 = AXIS2_PLACEMENT_3D('',#13683,#10774,#10775) ;
#9003 = AXIS2_PLACEMENT_3D('',#13684,#10776,#10777) ;
#9004 = AXIS2_PLACEMENT_3D('',#13685,#10778,#10779) ;
#9005 = AXIS2_PLACEMENT_3D('',#13686,#10780,#10781) ;
#9006 = AXIS2_PLACEMENT_3D('',#13687,#10782,#10783) ;
#9007 = AXIS2_PLACEMENT_3D('',#13688,#10784,#10785) ;
#9008 = AXIS2_PLACEMENT_3D('',#13689,#10786,#10787) ;
#9009 = AXIS2_PLACEMENT_3D('',#13690,#10788,#10789) ;
#9010 = AXIS2_PLACEMENT_3D('',#13691,#10790,#10791) ;
#9011 = AXIS2_PLACEMENT_3D('',#13692,#10792,#10793) ;
#9012 = AXIS2_PLACEMENT_3D('',#13693,#10794,#10795) ;
#9013 = AXIS2_PLACEMENT_3D('',#13695,#10796,#10797) ;
#9014 = AXIS2_PLACEMENT_3D('',#13698,#10799,#10800) ;
#9015 = AXIS2_PLACEMENT_3D('',#13699,#10801,#10802) ;
#9016 = AXIS2_PLACEMENT_3D('',#13708,#10807,#10808) ;
#9017 = AXIS2_PLACEMENT_3D('',#13714,#10812,#10813) ;
#9018 = AXIS2_PLACEMENT_3D('',#13720,#10817,#10818) ;
#9019 = AXIS2_PLACEMENT_3D('',#13724,#10820,#10821) ;
#9020 = AXIS2_PLACEMENT_3D('',#13732,#10825,#10826) ;
#9021 = AXIS2_PLACEMENT_3D('',#13735,#10828,#10829) ;
#9022 = AXIS2_PLACEMENT_3D('',#13736,#10830,#10831) ;
#9023 = AXIS2_PLACEMENT_3D('',#13740,#10834,#10835) ;
#9024 = AXIS2_PLACEMENT_3D('',#13743,#10837,#10838) ;
#9025 = AXIS2_PLACEMENT_3D('',#13744,#10839,#10840) ;
#9026 = AXIS2_PLACEMENT_3D('',#13746,#10841,#10842) ;
#9027 = AXIS2_PLACEMENT_3D('',#13748,#10844,#10845) ;
#9028 = AXIS2_PLACEMENT_3D('',#13753,#10848,#10849) ;
#9029 = AXIS2_PLACEMENT_3D('',#13754,#10850,#10851) ;
#9030 = AXIS2_PLACEMENT_3D('',#13758,#10854,#10855) ;
#9031 = AXIS2_PLACEMENT_3D('',#13760,#10857,#10858) ;
#9032 = AXIS2_PLACEMENT_3D('',#13764,#10861,#10862) ;
#9033 = AXIS2_PLACEMENT_3D('',#13766,#10864,#10865) ;
#9034 = AXIS2_PLACEMENT_3D('',#13767,#10866,#10867) ;
#9035 = AXIS2_PLACEMENT_3D('',#13768,#10868,#10869) ;
#9036 = AXIS2_PLACEMENT_3D('',#13770,#10870,#10871) ;
#9037 = AXIS2_PLACEMENT_3D('',#13772,#10872,#10873) ;
#9038 = AXIS2_PLACEMENT_3D('',#13773,#10874,#10875) ;
#9039 = AXIS2_PLACEMENT_3D('',#13776,#10877,#10878) ;
#9040 = AXIS2_PLACEMENT_3D('',#13777,#10879,#10880) ;
#9041 = AXIS2_PLACEMENT_3D('',#13778,#10881,#10882) ;
#9042 = AXIS2_PLACEMENT_3D('',#13780,#10883,#10884) ;
#9043 = AXIS2_PLACEMENT_3D('',#13782,#10886,#10887) ;
#9044 = AXIS2_PLACEMENT_3D('',#13783,#10888,#10889) ;
#9045 = AXIS2_PLACEMENT_3D('',#13784,#10890,#10891) ;
#9046 = AXIS2_PLACEMENT_3D('',#13787,#10892,#10893) ;
#9047 = AXIS2_PLACEMENT_3D('',#13788,#10894,#10895) ;
#9048 = AXIS2_PLACEMENT_3D('',#13789,#10896,#10897) ;
#9049 = AXIS2_PLACEMENT_3D('',#13792,#10898,#10899) ;
#9050 = AXIS2_PLACEMENT_3D('',#13794,#10900,#10901) ;
#9051 = AXIS2_PLACEMENT_3D('',#13795,#10902,#10903) ;
#9052 = AXIS2_PLACEMENT_3D('',#13796,#10904,#10905) ;
#9053 = AXIS2_PLACEMENT_3D('',#13799,#10906,#10907) ;
#9054 = AXIS2_PLACEMENT_3D('',#13801,#10908,#10909) ;
#9055 = AXIS2_PLACEMENT_3D('',#13803,#10910,#10911) ;
#9056 = AXIS2_PLACEMENT_3D('',#13804,#10912,#10913) ;
#9057 = AXIS2_PLACEMENT_3D('',#13805,#10914,#10915) ;
#9058 = AXIS2_PLACEMENT_3D('',#13808,#10916,#10917) ;
#9059 = AXIS2_PLACEMENT_3D('',#13810,#10918,#10919) ;
#9060 = AXIS2_PLACEMENT_3D('',#13812,#10920,#10921) ;
#9061 = AXIS2_PLACEMENT_3D('',#13813,#10922,#10923) ;
#9062 = AXIS2_PLACEMENT_3D('',#13814,#10924,#10925) ;
#9063 = AXIS2_PLACEMENT_3D('',#13817,#10926,#10927) ;
#9064 = AXIS2_PLACEMENT_3D('',#13819,#10928,#10929) ;
#9065 = AXIS2_PLACEMENT_3D('',#13821,#10930,#10931) ;
#9066 = AXIS2_PLACEMENT_3D('',#13822,#10932,#10933) ;
#9067 = AXIS2_PLACEMENT_3D('',#13823,#10934,#10935) ;
#9068 = AXIS2_PLACEMENT_3D('',#13826,#10936,#10937) ;
#9069 = AXIS2_PLACEMENT_3D('',#13828,#10938,#10939) ;
#9070 = AXIS2_PLACEMENT_3D('',#13829,#10940,#10941) ;
#9071 = AXIS2_PLACEMENT_3D('',#13830,#10942,#10943) ;
#9072 = AXIS2_PLACEMENT_3D('',#13833,#10944,#10945) ;
#9073 = AXIS2_PLACEMENT_3D('',#13834,#10946,#10947) ;
#9074 = AXIS2_PLACEMENT_3D('',#13835,#10948,#10949) ;
#9075 = AXIS2_PLACEMENT_3D('',#13838,#10950,#10951) ;
#9076 = AXIS2_PLACEMENT_3D('',#13839,#10952,#10953) ;
#9077 = AXIS2_PLACEMENT_3D('',#13840,#10954,#10955) ;
#9078 = AXIS2_PLACEMENT_3D('',#13843,#10956,#10957) ;
#9079 = AXIS2_PLACEMENT_3D('',#13844,#10958,#10959) ;
#9080 = AXIS2_PLACEMENT_3D('',#13845,#10960,#10961) ;
#9081 = AXIS2_PLACEMENT_3D('',#13848,#10962,#10963) ;
#9082 = AXIS2_PLACEMENT_3D('',#13850,#10964,#10965) ;
#9083 = AXIS2_PLACEMENT_3D('',#13851,#10966,#10967) ;
#9084 = AXIS2_PLACEMENT_3D('',#13852,#10968,#10969) ;
#9085 = AXIS2_PLACEMENT_3D('',#13855,#10970,#10971) ;
#9086 = AXIS2_PLACEMENT_3D('',#13857,#10972,#10973) ;
#9087 = AXIS2_PLACEMENT_3D('',#13859,#10974,#10975) ;
#9088 = AXIS2_PLACEMENT_3D('',#13860,#10976,#10977) ;
#9089 = AXIS2_PLACEMENT_3D('',#13861,#10978,#10979) ;
#9090 = AXIS2_PLACEMENT_3D('',#13864,#10980,#10981) ;
#9091 = AXIS2_PLACEMENT_3D('',#13866,#10982,#10983) ;
#9092 = AXIS2_PLACEMENT_3D('',#13868,#10984,#10985) ;
#9093 = AXIS2_PLACEMENT_3D('',#13869,#10986,#10987) ;
#9094 = AXIS2_PLACEMENT_3D('',#13870,#10988,#10989) ;
#9095 = AXIS2_PLACEMENT_3D('',#13873,#10990,#10991) ;
#9096 = AXIS2_PLACEMENT_3D('',#13875,#10992,#10993) ;
#9097 = AXIS2_PLACEMENT_3D('',#13877,#10994,#10995) ;
#9098 = AXIS2_PLACEMENT_3D('',#13878,#10996,#10997) ;
#9099 = AXIS2_PLACEMENT_3D('',#13879,#10998,#10999) ;
#9100 = AXIS2_PLACEMENT_3D('',#13882,#11000,#11001) ;
#9101 = AXIS2_PLACEMENT_3D('',#13884,#11002,#11003) ;
#9102 = AXIS2_PLACEMENT_3D('',#13885,#11004,#11005) ;
#9103 = AXIS2_PLACEMENT_3D('',#13886,#11006,#11007) ;
#9104 = AXIS2_PLACEMENT_3D('',#13889,#11008,#11009) ;
#9105 = AXIS2_PLACEMENT_3D('',#13890,#11010,#11011) ;
#9106 = AXIS2_PLACEMENT_3D('',#13891,#11012,#11013) ;
#9107 = AXIS2_PLACEMENT_3D('',#13894,#11014,#11015) ;
#9108 = AXIS2_PLACEMENT_3D('',#13895,#11016,#11017) ;
#9109 = AXIS2_PLACEMENT_3D('',#13896,#11018,#11019) ;
#9110 = AXIS2_PLACEMENT_3D('',#13899,#11020,#11021) ;
#9111 = AXIS2_PLACEMENT_3D('',#13900,#11022,#11023) ;
#9112 = AXIS2_PLACEMENT_3D('',#13901,#11024,#11025) ;
#9113 = AXIS2_PLACEMENT_3D('',#13904,#11026,#11027) ;
#9114 = AXIS2_PLACEMENT_3D('',#13906,#11028,#11029) ;
#9115 = AXIS2_PLACEMENT_3D('',#13907,#11030,#11031) ;
#9116 = AXIS2_PLACEMENT_3D('',#13908,#11032,#11033) ;
#9117 = AXIS2_PLACEMENT_3D('',#13911,#11034,#11035) ;
#9118 = AXIS2_PLACEMENT_3D('',#13913,#11036,#11037) ;
#9119 = AXIS2_PLACEMENT_3D('',#13915,#11038,#11039) ;
#9120 = AXIS2_PLACEMENT_3D('',#13916,#11040,#11041) ;
#9121 = AXIS2_PLACEMENT_3D('',#13917,#11042,#11043) ;
#9122 = AXIS2_PLACEMENT_3D('',#13920,#11044,#11045) ;
#9123 = AXIS2_PLACEMENT_3D('',#13922,#11046,#11047) ;
#9124 = AXIS2_PLACEMENT_3D('',#13924,#11048,#11049) ;
#9125 = AXIS2_PLACEMENT_3D('',#13925,#11050,#11051) ;
#9126 = AXIS2_PLACEMENT_3D('',#13926,#11052,#11053) ;
#9127 = AXIS2_PLACEMENT_3D('',#13929,#11054,#11055) ;
#9128 = AXIS2_PLACEMENT_3D('',#13931,#11056,#11057) ;
#9129 = AXIS2_PLACEMENT_3D('',#13933,#11058,#11059) ;
#9130 = AXIS2_PLACEMENT_3D('',#13934,#11060,#11061) ;
#9131 = AXIS2_PLACEMENT_3D('',#13935,#11062,#11063) ;
#9132 = AXIS2_PLACEMENT_3D('',#13938,#11064,#11065) ;
#9133 = AXIS2_PLACEMENT_3D('',#13940,#11066,#11067) ;
#9134 = AXIS2_PLACEMENT_3D('',#13941,#11068,#11069) ;
#9135 = AXIS2_PLACEMENT_3D('',#13942,#11070,#11071) ;
#9136 = AXIS2_PLACEMENT_3D('',#13945,#11072,#11073) ;
#9137 = AXIS2_PLACEMENT_3D('',#13946,#11074,#11075) ;
#9138 = AXIS2_PLACEMENT_3D('',#13947,#11076,#11077) ;
#9139 = AXIS2_PLACEMENT_3D('',#13950,#11078,#11079) ;
#9140 = AXIS2_PLACEMENT_3D('',#13951,#11080,#11081) ;
#9141 = AXIS2_PLACEMENT_3D('',#13952,#11082,#11083) ;
#9142 = AXIS2_PLACEMENT_3D('',#13955,#11084,#11085) ;
#9143 = AXIS2_PLACEMENT_3D('',#13956,#11086,#11087) ;
#9144 = AXIS2_PLACEMENT_3D('',#13957,#11088,#11089) ;
#9145 = AXIS2_PLACEMENT_3D('',#13960,#11090,#11091) ;
#9146 = AXIS2_PLACEMENT_3D('',#13962,#11092,#11093) ;
#9147 = AXIS2_PLACEMENT_3D('',#13963,#11094,#11095) ;
#9148 = AXIS2_PLACEMENT_3D('',#13964,#11096,#11097) ;
#9149 = AXIS2_PLACEMENT_3D('',#13967,#11098,#11099) ;
#9150 = AXIS2_PLACEMENT_3D('',#13969,#11100,#11101) ;
#9151 = AXIS2_PLACEMENT_3D('',#13971,#11102,#11103) ;
#9152 = AXIS2_PLACEMENT_3D('',#13972,#11104,#11105) ;
#9153 = AXIS2_PLACEMENT_3D('',#13973,#11106,#11107) ;
#9154 = AXIS2_PLACEMENT_3D('',#13976,#11108,#11109) ;
#9155 = AXIS2_PLACEMENT_3D('',#13978,#11110,#11111) ;
#9156 = AXIS2_PLACEMENT_3D('',#13980,#11112,#11113) ;
#9157 = AXIS2_PLACEMENT_3D('',#13981,#11114,#11115) ;
#9158 = AXIS2_PLACEMENT_3D('',#13982,#11116,#11117) ;
#9159 = AXIS2_PLACEMENT_3D('',#13985,#11118,#11119) ;
#9160 = AXIS2_PLACEMENT_3D('',#13987,#11120,#11121) ;
#9161 = AXIS2_PLACEMENT_3D('',#13989,#11122,#11123) ;
#9162 = AXIS2_PLACEMENT_3D('',#13990,#11124,#11125) ;
#9163 = AXIS2_PLACEMENT_3D('',#13991,#11126,#11127) ;
#9164 = AXIS2_PLACEMENT_3D('',#13994,#11128,#11129) ;
#9165 = AXIS2_PLACEMENT_3D('',#13996,#11130,#11131) ;
#9166 = AXIS2_PLACEMENT_3D('',#13997,#11132,#11133) ;
#9167 = AXIS2_PLACEMENT_3D('',#13998,#11134,#11135) ;
#9168 = AXIS2_PLACEMENT_3D('',#14001,#11136,#11137) ;
#9169 = AXIS2_PLACEMENT_3D('',#14002,#11138,#11139) ;
#9170 = AXIS2_PLACEMENT_3D('',#14003,#11140,#11141) ;
#9171 = AXIS2_PLACEMENT_3D('',#14006,#11142,#11143) ;
#9172 = AXIS2_PLACEMENT_3D('',#14007,#11144,#11145) ;
#9173 = AXIS2_PLACEMENT_3D('',#14008,#11146,#11147) ;
#9174 = AXIS2_PLACEMENT_3D('',#14011,#11148,#11149) ;
#9175 = AXIS2_PLACEMENT_3D('',#14012,#11150,#11151) ;
#9176 = AXIS2_PLACEMENT_3D('',#14013,#11152,#11153) ;
#9177 = AXIS2_PLACEMENT_3D('',#14016,#11154,#11155) ;
#9178 = AXIS2_PLACEMENT_3D('',#14018,#11156,#11157) ;
#9179 = AXIS2_PLACEMENT_3D('',#14019,#11158,#11159) ;
#9180 = AXIS2_PLACEMENT_3D('',#14020,#11160,#11161) ;
#9181 = AXIS2_PLACEMENT_3D('',#14023,#11162,#11163) ;
#9182 = AXIS2_PLACEMENT_3D('',#14025,#11164,#11165) ;
#9183 = AXIS2_PLACEMENT_3D('',#14027,#11166,#11167) ;
#9184 = AXIS2_PLACEMENT_3D('',#14028,#11168,#11169) ;
#9185 = AXIS2_PLACEMENT_3D('',#14029,#11170,#11171) ;
#9186 = AXIS2_PLACEMENT_3D('',#14032,#11172,#11173) ;
#9187 = AXIS2_PLACEMENT_3D('',#14034,#11174,#11175) ;
#9188 = AXIS2_PLACEMENT_3D('',#14036,#11176,#11177) ;
#9189 = AXIS2_PLACEMENT_3D('',#14037,#11178,#11179) ;
#9190 = AXIS2_PLACEMENT_3D('',#14038,#11180,#11181) ;
#9191 = AXIS2_PLACEMENT_3D('',#14041,#11182,#11183) ;
#9192 = AXIS2_PLACEMENT_3D('',#14043,#11184,#11185) ;
#9193 = AXIS2_PLACEMENT_3D('',#14045,#11186,#11187) ;
#9194 = AXIS2_PLACEMENT_3D('',#14046,#11188,#11189) ;
#9195 = AXIS2_PLACEMENT_3D('',#14047,#11190,#11191) ;
#9196 = AXIS2_PLACEMENT_3D('',#14050,#11192,#11193) ;
#9197 = AXIS2_PLACEMENT_3D('',#14052,#11194,#11195) ;
#9198 = AXIS2_PLACEMENT_3D('',#14053,#11196,#11197) ;
#9199 = AXIS2_PLACEMENT_3D('',#14054,#11198,#11199) ;
#9200 = AXIS2_PLACEMENT_3D('',#14057,#11200,#11201) ;
#9201 = AXIS2_PLACEMENT_3D('',#14058,#11202,#11203) ;
#9202 = AXIS2_PLACEMENT_3D('',#14059,#11204,#11205) ;
#9203 = AXIS2_PLACEMENT_3D('',#14061,#11206,#11207) ;
#9204 = AXIS2_PLACEMENT_3D('',#14065,#11209,#11210) ;
#9205 = AXIS2_PLACEMENT_3D('',#14066,#11211,#11212) ;
#9206 = AXIS2_PLACEMENT_3D('',#14067,#11213,#11214) ;
#9207 = AXIS2_PLACEMENT_3D('',#14068,#11215,#11216) ;
#9208 = AXIS2_PLACEMENT_3D('',#14069,#11217,#11218) ;
#9209 = AXIS2_PLACEMENT_3D('',#14072,#11220,#11221) ;
#9210 = AXIS2_PLACEMENT_3D('',#14073,#11222,#11223) ;
#9211 = AXIS2_PLACEMENT_3D('',#14074,#11224,#11225) ;
#9212 = AXIS2_PLACEMENT_3D('',#14076,#11227,#11228) ;
#9213 = AXIS2_PLACEMENT_3D('',#14077,#11229,#11230) ;
#9214 = AXIS2_PLACEMENT_3D('',#14079,#11232,#11233) ;
#9215 = AXIS2_PLACEMENT_3D('',#14080,#11234,#11235) ;
#9216 = AXIS2_PLACEMENT_3D('',#14082,#11237,#11238) ;
#9217 = AXIS2_PLACEMENT_3D('',#14083,#11239,#11240) ;
#9218 = AXIS2_PLACEMENT_3D('',#14086,#11242,#11243) ;
#9219 = AXIS2_PLACEMENT_3D('',#14087,#11244,#11245) ;
#9220 = AXIS2_PLACEMENT_3D('',#14088,#11246,#11247) ;
#9221 = AXIS2_PLACEMENT_3D('',#14092,#11249,#11250) ;
#9222 = AXIS2_PLACEMENT_3D('',#14093,#11251,#11252) ;
#9223 = AXIS2_PLACEMENT_3D('',#14094,#11253,#11254) ;
#9224 = AXIS2_PLACEMENT_3D('',#14095,#11255,#11256) ;
#9225 = AXIS2_PLACEMENT_3D('',#14098,#11258,#11259) ;
#9226 = AXIS2_PLACEMENT_3D('',#14099,#11260,#11261) ;
#9227 = AXIS2_PLACEMENT_3D('',#14100,#11262,#11263) ;
#9228 = AXIS2_PLACEMENT_3D('',#14104,#11265,#11266) ;
#9229 = AXIS2_PLACEMENT_3D('',#14105,#11267,#11268) ;
#9230 = AXIS2_PLACEMENT_3D('',#14106,#11269,#11270) ;
#9231 = AXIS2_PLACEMENT_3D('',#14107,#11271,#11272) ;
#9232 = AXIS2_PLACEMENT_3D('',#14110,#11274,#11275) ;
#9233 = AXIS2_PLACEMENT_3D('',#14111,#11276,#11277) ;
#9234 = AXIS2_PLACEMENT_3D('',#14112,#11278,#11279) ;
#9235 = AXIS2_PLACEMENT_3D('',#14114,#11281,#11282) ;
#9236 = AXIS2_PLACEMENT_3D('',#14115,#11283,#11284) ;
#9237 = AXIS2_PLACEMENT_3D('',#14117,#11286,#11287) ;
#9238 = AXIS2_PLACEMENT_3D('',#14118,#11288,#11289) ;
#9239 = AXIS2_PLACEMENT_3D('',#14120,#11291,#11292) ;
#9240 = AXIS2_PLACEMENT_3D('',#14121,#11293,#11294) ;
#9241 = AXIS2_PLACEMENT_3D('',#14124,#11296,#11297) ;
#9242 = AXIS2_PLACEMENT_3D('',#14125,#11298,#11299) ;
#9243 = AXIS2_PLACEMENT_3D('',#14126,#11300,#11301) ;
#9244 = AXIS2_PLACEMENT_3D('',#14130,#11303,#11304) ;
#9245 = AXIS2_PLACEMENT_3D('',#14131,#11305,#11306) ;
#9246 = AXIS2_PLACEMENT_3D('',#14132,#11307,#11308) ;
#9247 = AXIS2_PLACEMENT_3D('',#14133,#11309,#11310) ;
#9248 = AXIS2_PLACEMENT_3D('',#14136,#11312,#11313) ;
#9249 = AXIS2_PLACEMENT_3D('',#14137,#11314,#11315) ;
#9250 = AXIS2_PLACEMENT_3D('',#14138,#11316,#11317) ;
#9251 = AXIS2_PLACEMENT_3D('',#14142,#11319,#11320) ;
#9252 = AXIS2_PLACEMENT_3D('',#14143,#11321,#11322) ;
#9253 = AXIS2_PLACEMENT_3D('',#14144,#11323,#11324) ;
#9254 = AXIS2_PLACEMENT_3D('',#14145,#11325,#11326) ;
#9255 = AXIS2_PLACEMENT_3D('',#14148,#11328,#11329) ;
#9256 = AXIS2_PLACEMENT_3D('',#14149,#11330,#11331) ;
#9257 = AXIS2_PLACEMENT_3D('',#14150,#11332,#11333) ;
#9258 = AXIS2_PLACEMENT_3D('',#14152,#11335,#11336) ;
#9259 = AXIS2_PLACEMENT_3D('',#14153,#11337,#11338) ;
#9260 = AXIS2_PLACEMENT_3D('',#14155,#11340,#11341) ;
#9261 = AXIS2_PLACEMENT_3D('',#14156,#11342,#11343) ;
#9262 = AXIS2_PLACEMENT_3D('',#14158,#11345,#11346) ;
#9263 = AXIS2_PLACEMENT_3D('',#14159,#11347,#11348) ;
#9264 = AXIS2_PLACEMENT_3D('',#14162,#11350,#11351) ;
#9265 = AXIS2_PLACEMENT_3D('',#14163,#11352,#11353) ;
#9266 = AXIS2_PLACEMENT_3D('',#14164,#11354,#11355) ;
#9267 = AXIS2_PLACEMENT_3D('',#14168,#11357,#11358) ;
#9268 = AXIS2_PLACEMENT_3D('',#14169,#11359,#11360) ;
#9269 = AXIS2_PLACEMENT_3D('',#14170,#11361,#11362) ;
#9270 = AXIS2_PLACEMENT_3D('',#14171,#11363,#11364) ;
#9271 = AXIS2_PLACEMENT_3D('',#14174,#11366,#11367) ;
#9272 = AXIS2_PLACEMENT_3D('',#14175,#11368,#11369) ;
#9273 = AXIS2_PLACEMENT_3D('',#14176,#11370,#11371) ;
#9274 = AXIS2_PLACEMENT_3D('',#14180,#11373,#11374) ;
#9275 = AXIS2_PLACEMENT_3D('',#14181,#11375,#11376) ;
#9276 = AXIS2_PLACEMENT_3D('',#14182,#11377,#11378) ;
#9277 = AXIS2_PLACEMENT_3D('',#14183,#11379,#11380) ;
#9278 = AXIS2_PLACEMENT_3D('',#14186,#11382,#11383) ;
#9279 = AXIS2_PLACEMENT_3D('',#14187,#11384,#11385) ;
#9280 = AXIS2_PLACEMENT_3D('',#14188,#11386,#11387) ;
#9281 = AXIS2_PLACEMENT_3D('',#14190,#11389,#11390) ;
#9282 = AXIS2_PLACEMENT_3D('',#14191,#11391,#11392) ;
#9283 = AXIS2_PLACEMENT_3D('',#14193,#11394,#11395) ;
#9284 = AXIS2_PLACEMENT_3D('',#14194,#11396,#11397) ;
#9285 = AXIS2_PLACEMENT_3D('',#14196,#11399,#11400) ;
#9286 = AXIS2_PLACEMENT_3D('',#14197,#11401,#11402) ;
#9287 = AXIS2_PLACEMENT_3D('',#14200,#11404,#11405) ;
#9288 = AXIS2_PLACEMENT_3D('',#14201,#11406,#11407) ;
#9289 = AXIS2_PLACEMENT_3D('',#14202,#11408,#11409) ;
#9290 = AXIS2_PLACEMENT_3D('',#14206,#11411,#11412) ;
#9291 = AXIS2_PLACEMENT_3D('',#14207,#11413,#11414) ;
#9292 = AXIS2_PLACEMENT_3D('',#14208,#11415,#11416) ;
#9293 = AXIS2_PLACEMENT_3D('',#14209,#11417,#11418) ;
#9294 = AXIS2_PLACEMENT_3D('',#14212,#11420,#11421) ;
#9295 = AXIS2_PLACEMENT_3D('',#14213,#11422,#11423) ;
#9296 = AXIS2_PLACEMENT_3D('',#14214,#11424,#11425) ;
#9297 = AXIS2_PLACEMENT_3D('',#14218,#11427,#11428) ;
#9298 = AXIS2_PLACEMENT_3D('',#14219,#11429,#11430) ;
#9299 = AXIS2_PLACEMENT_3D('',#14220,#11431,#11432) ;
#9300 = AXIS2_PLACEMENT_3D('',#14221,#11433,#11434) ;
#9301 = AXIS2_PLACEMENT_3D('',#14224,#11436,#11437) ;
#9302 = AXIS2_PLACEMENT_3D('',#14225,#11438,#11439) ;
#9303 = AXIS2_PLACEMENT_3D('',#14226,#11440,#11441) ;
#9304 = AXIS2_PLACEMENT_3D('',#14228,#11443,#11444) ;
#9305 = AXIS2_PLACEMENT_3D('',#14229,#11445,#11446) ;
#9306 = AXIS2_PLACEMENT_3D('',#14231,#11448,#11449) ;
#9307 = AXIS2_PLACEMENT_3D('',#14232,#11450,#11451) ;
#9308 = AXIS2_PLACEMENT_3D('',#14234,#11453,#11454) ;
#9309 = AXIS2_PLACEMENT_3D('',#14235,#11455,#11456) ;
#9310 = AXIS2_PLACEMENT_3D('',#14238,#11458,#11459) ;
#9311 = AXIS2_PLACEMENT_3D('',#14239,#11460,#11461) ;
#9312 = AXIS2_PLACEMENT_3D('',#14240,#11462,#11463) ;
#9313 = AXIS2_PLACEMENT_3D('',#14244,#11465,#11466) ;
#9314 = AXIS2_PLACEMENT_3D('',#14245,#11467,#11468) ;
#9315 = AXIS2_PLACEMENT_3D('',#14246,#11469,#11470) ;
#9316 = AXIS2_PLACEMENT_3D('',#14247,#11471,#11472) ;
#9317 = AXIS2_PLACEMENT_3D('',#14250,#11474,#11475) ;
#9318 = AXIS2_PLACEMENT_3D('',#14251,#11476,#11477) ;
#9319 = AXIS2_PLACEMENT_3D('',#14252,#11478,#11479) ;
#9320 = AXIS2_PLACEMENT_3D('',#14253,#11480,#11481) ;
#9321 = AXIS2_PLACEMENT_3D('',#14255,#11482,#11483) ;
#9322 = AXIS2_PLACEMENT_3D('',#14257,#11484,#11485) ;
#9323 = AXIS2_PLACEMENT_3D('',#14258,#11486,#11487) ;
#9324 = AXIS2_PLACEMENT_3D('',#14260,#11488,#11489) ;
#9325 = AXIS2_PLACEMENT_3D('',#14262,#11490,#11491) ;
#9326 = AXIS2_PLACEMENT_3D('',#14263,#11492,#11493) ;
#9327 = AXIS2_PLACEMENT_3D('',#14265,#11495,#11496) ;
#9328 = AXIS2_PLACEMENT_3D('',#14267,#11497,#11498) ;
#9329 = AXIS2_PLACEMENT_3D('',#14269,#11500,#11501) ;
#9330 = AXIS2_PLACEMENT_3D('',#14272,#11503,#11504) ;
#9331 = AXIS2_PLACEMENT_3D('',#14273,#11505,#11506) ;
#9332 = AXIS2_PLACEMENT_3D('',#14274,#11507,#11508) ;
#9333 = AXIS2_PLACEMENT_3D('',#14275,#11509,#11510) ;
#9334 = AXIS2_PLACEMENT_3D('',#14276,#11511,#11512) ;
#9335 = AXIS2_PLACEMENT_3D('',#14285,#11517,#11518) ;
#9336 = AXIS2_PLACEMENT_3D('',#14291,#11522,#11523) ;
#9337 = AXIS2_PLACEMENT_3D('',#14295,#11526,#11527) ;
#9338 = AXIS2_PLACEMENT_3D('',#14299,#11530,#11531) ;
#9339 = AXIS2_PLACEMENT_3D('',#14301,#11533,#11534) ;
#9340 = AXIS2_PLACEMENT_3D('',#14303,#11535,#11536) ;
#9341 = AXIS2_PLACEMENT_3D('',#14306,#11538,#11539) ;
#9342 = AXIS2_PLACEMENT_3D('',#14307,#11540,#11541) ;
#9343 = AXIS2_PLACEMENT_3D('',#14308,#11542,#11543) ;
#9344 = AXIS2_PLACEMENT_3D('',#14317,#11548,#11549) ;
#9345 = AXIS2_PLACEMENT_3D('',#14326,#11554,#11555) ;
#9346 = AXIS2_PLACEMENT_3D('',#14329,#11558,#11559) ;
#9347 = AXIS2_PLACEMENT_3D('',#14331,#11561,#11562) ;
#9348 = AXIS2_PLACEMENT_3D('',#14333,#11564,#11565) ;
#9349 = AXIS2_PLACEMENT_3D('',#14334,#11566,#11567) ;
#9350 = AXIS2_PLACEMENT_3D('',#14335,#11568,#11569) ;
#9351 = AXIS2_PLACEMENT_3D('',#14338,#11570,#11571) ;
#9352 = AXIS2_PLACEMENT_3D('',#14339,#11572,#11573) ;
#9353 = AXIS2_PLACEMENT_3D('',#14340,#11574,#11575) ;
#9354 = AXIS2_PLACEMENT_3D('',#14343,#11576,#11577) ;
#9355 = AXIS2_PLACEMENT_3D('',#14345,#11578,#11579) ;
#9356 = AXIS2_PLACEMENT_3D('',#14346,#11580,#11581) ;
#9357 = AXIS2_PLACEMENT_3D('',#14347,#11582,#11583) ;
#9358 = AXIS2_PLACEMENT_3D('',#14350,#11584,#11585) ;
#9359 = AXIS2_PLACEMENT_3D('',#14352,#11586,#11587) ;
#9360 = AXIS2_PLACEMENT_3D('',#14354,#11588,#11589) ;
#9361 = AXIS2_PLACEMENT_3D('',#14355,#11590,#11591) ;
#9362 = AXIS2_PLACEMENT_3D('',#14356,#11592,#11593) ;
#9363 = AXIS2_PLACEMENT_3D('',#14359,#11594,#11595) ;
#9364 = AXIS2_PLACEMENT_3D('',#14361,#11596,#11597) ;
#9365 = AXIS2_PLACEMENT_3D('',#14363,#11598,#11599) ;
#9366 = AXIS2_PLACEMENT_3D('',#14364,#11600,#11601) ;
#9367 = AXIS2_PLACEMENT_3D('',#14365,#11602,#11603) ;
#9368 = AXIS2_PLACEMENT_3D('',#14368,#11604,#11605) ;
#9369 = AXIS2_PLACEMENT_3D('',#14370,#11606,#11607) ;
#9370 = AXIS2_PLACEMENT_3D('',#14372,#11608,#11609) ;
#9371 = AXIS2_PLACEMENT_3D('',#14373,#11610,#11611) ;
#9372 = AXIS2_PLACEMENT_3D('',#14374,#11612,#11613) ;
#9373 = AXIS2_PLACEMENT_3D('',#14377,#11614,#11615) ;
#9374 = AXIS2_PLACEMENT_3D('',#14379,#11616,#11617) ;
#9375 = AXIS2_PLACEMENT_3D('',#14380,#11618,#11619) ;
#9376 = AXIS2_PLACEMENT_3D('',#14381,#11620,#11621) ;
#9377 = AXIS2_PLACEMENT_3D('',#14384,#11622,#11623) ;
#9378 = AXIS2_PLACEMENT_3D('',#14385,#11624,#11625) ;
#9379 = AXIS2_PLACEMENT_3D('',#14386,#11626,#11627) ;
#9380 = AXIS2_PLACEMENT_3D('',#14389,#11628,#11629) ;
#9381 = AXIS2_PLACEMENT_3D('',#14390,#11630,#11631) ;
#9382 = AXIS2_PLACEMENT_3D('',#14391,#11632,#11633) ;
#9383 = AXIS2_PLACEMENT_3D('',#14394,#11634,#11635) ;
#9384 = AXIS2_PLACEMENT_3D('',#14395,#11636,#11637) ;
#9385 = AXIS2_PLACEMENT_3D('',#14396,#11638,#11639) ;
#9386 = AXIS2_PLACEMENT_3D('',#14399,#11640,#11641) ;
#9387 = AXIS2_PLACEMENT_3D('',#14401,#11642,#11643) ;
#9388 = AXIS2_PLACEMENT_3D('',#14402,#11644,#11645) ;
#9389 = AXIS2_PLACEMENT_3D('',#14403,#11646,#11647) ;
#9390 = AXIS2_PLACEMENT_3D('',#14406,#11648,#11649) ;
#9391 = AXIS2_PLACEMENT_3D('',#14408,#11650,#11651) ;
#9392 = AXIS2_PLACEMENT_3D('',#14410,#11652,#11653) ;
#9393 = AXIS2_PLACEMENT_3D('',#14411,#11654,#11655) ;
#9394 = AXIS2_PLACEMENT_3D('',#14412,#11656,#11657) ;
#9395 = AXIS2_PLACEMENT_3D('',#14415,#11658,#11659) ;
#9396 = AXIS2_PLACEMENT_3D('',#14417,#11660,#11661) ;
#9397 = AXIS2_PLACEMENT_3D('',#14419,#11662,#11663) ;
#9398 = AXIS2_PLACEMENT_3D('',#14420,#11664,#11665) ;
#9399 = AXIS2_PLACEMENT_3D('',#14421,#11666,#11667) ;
#9400 = AXIS2_PLACEMENT_3D('',#14424,#11668,#11669) ;
#9401 = AXIS2_PLACEMENT_3D('',#14426,#11670,#11671) ;
#9402 = AXIS2_PLACEMENT_3D('',#14428,#11672,#11673) ;
#9403 = AXIS2_PLACEMENT_3D('',#14429,#11674,#11675) ;
#9404 = AXIS2_PLACEMENT_3D('',#14430,#11676,#11677) ;
#9405 = AXIS2_PLACEMENT_3D('',#14433,#11678,#11679) ;
#9406 = AXIS2_PLACEMENT_3D('',#14435,#11680,#11681) ;
#9407 = AXIS2_PLACEMENT_3D('',#14436,#11682,#11683) ;
#9408 = AXIS2_PLACEMENT_3D('',#14437,#11684,#11685) ;
#9409 = AXIS2_PLACEMENT_3D('',#14440,#11686,#11687) ;
#9410 = AXIS2_PLACEMENT_3D('',#14441,#11688,#11689) ;
#9411 = AXIS2_PLACEMENT_3D('',#14442,#11690,#11691) ;
#9412 = AXIS2_PLACEMENT_3D('',#14445,#11692,#11693) ;
#9413 = AXIS2_PLACEMENT_3D('',#14446,#11694,#11695) ;
#9414 = AXIS2_PLACEMENT_3D('',#14447,#11696,#11697) ;
#9415 = AXIS2_PLACEMENT_3D('',#14450,#11698,#11699) ;
#9416 = AXIS2_PLACEMENT_3D('',#14451,#11700,#11701) ;
#9417 = AXIS2_PLACEMENT_3D('',#14452,#11702,#11703) ;
#9418 = AXIS2_PLACEMENT_3D('',#14455,#11704,#11705) ;
#9419 = AXIS2_PLACEMENT_3D('',#14457,#11706,#11707) ;
#9420 = AXIS2_PLACEMENT_3D('',#14458,#11708,#11709) ;
#9421 = AXIS2_PLACEMENT_3D('',#14459,#11710,#11711) ;
#9422 = AXIS2_PLACEMENT_3D('',#14462,#11712,#11713) ;
#9423 = AXIS2_PLACEMENT_3D('',#14464,#11714,#11715) ;
#9424 = AXIS2_PLACEMENT_3D('',#14466,#11716,#11717) ;
#9425 = AXIS2_PLACEMENT_3D('',#14467,#11718,#11719) ;
#9426 = AXIS2_PLACEMENT_3D('',#14468,#11720,#11721) ;
#9427 = AXIS2_PLACEMENT_3D('',#14471,#11722,#11723) ;
#9428 = AXIS2_PLACEMENT_3D('',#14473,#11724,#11725) ;
#9429 = AXIS2_PLACEMENT_3D('',#14475,#11726,#11727) ;
#9430 = AXIS2_PLACEMENT_3D('',#14476,#11728,#11729) ;
#9431 = AXIS2_PLACEMENT_3D('',#14477,#11730,#11731) ;
#9432 = AXIS2_PLACEMENT_3D('',#14480,#11732,#11733) ;
#9433 = AXIS2_PLACEMENT_3D('',#14482,#11734,#11735) ;
#9434 = AXIS2_PLACEMENT_3D('',#14484,#11736,#11737) ;
#9435 = AXIS2_PLACEMENT_3D('',#14485,#11738,#11739) ;
#9436 = AXIS2_PLACEMENT_3D('',#14486,#11740,#11741) ;
#9437 = AXIS2_PLACEMENT_3D('',#14489,#11742,#11743) ;
#9438 = AXIS2_PLACEMENT_3D('',#14491,#11744,#11745) ;
#9439 = AXIS2_PLACEMENT_3D('',#14492,#11746,#11747) ;
#9440 = AXIS2_PLACEMENT_3D('',#14493,#11748,#11749) ;
#9441 = AXIS2_PLACEMENT_3D('',#14496,#11750,#11751) ;
#9442 = AXIS2_PLACEMENT_3D('',#14497,#11752,#11753) ;
#9443 = AXIS2_PLACEMENT_3D('',#14498,#11754,#11755) ;
#9444 = AXIS2_PLACEMENT_3D('',#14500,#11756,#11757) ;
#9445 = AXIS2_PLACEMENT_3D('',#14504,#11759,#11760) ;
#9446 = AXIS2_PLACEMENT_3D('',#14505,#11761,#11762) ;
#9447 = AXIS2_PLACEMENT_3D('',#14506,#11763,#11764) ;
#9448 = AXIS2_PLACEMENT_3D('',#14507,#11765,#11766) ;
#9449 = AXIS2_PLACEMENT_3D('',#14508,#11767,#11768) ;
#9450 = AXIS2_PLACEMENT_3D('',#14511,#11770,#11771) ;
#9451 = AXIS2_PLACEMENT_3D('',#14512,#11772,#11773) ;
#9452 = AXIS2_PLACEMENT_3D('',#14513,#11774,#11775) ;
#9453 = AXIS2_PLACEMENT_3D('',#14515,#11777,#11778) ;
#9454 = AXIS2_PLACEMENT_3D('',#14516,#11779,#11780) ;
#9455 = AXIS2_PLACEMENT_3D('',#14518,#11782,#11783) ;
#9456 = AXIS2_PLACEMENT_3D('',#14519,#11784,#11785) ;
#9457 = AXIS2_PLACEMENT_3D('',#14521,#11787,#11788) ;
#9458 = AXIS2_PLACEMENT_3D('',#14522,#11789,#11790) ;
#9459 = AXIS2_PLACEMENT_3D('',#14525,#11792,#11793) ;
#9460 = AXIS2_PLACEMENT_3D('',#14526,#11794,#11795) ;
#9461 = AXIS2_PLACEMENT_3D('',#14527,#11796,#11797) ;
#9462 = AXIS2_PLACEMENT_3D('',#14531,#11799,#11800) ;
#9463 = AXIS2_PLACEMENT_3D('',#14532,#11801,#11802) ;
#9464 = AXIS2_PLACEMENT_3D('',#14533,#11803,#11804) ;
#9465 = AXIS2_PLACEMENT_3D('',#14534,#11805,#11806) ;
#9466 = AXIS2_PLACEMENT_3D('',#14537,#11808,#11809) ;
#9467 = AXIS2_PLACEMENT_3D('',#14538,#11810,#11811) ;
#9468 = AXIS2_PLACEMENT_3D('',#14539,#11812,#11813) ;
#9469 = AXIS2_PLACEMENT_3D('',#14543,#11815,#11816) ;
#9470 = AXIS2_PLACEMENT_3D('',#14544,#11817,#11818) ;
#9471 = AXIS2_PLACEMENT_3D('',#14545,#11819,#11820) ;
#9472 = AXIS2_PLACEMENT_3D('',#14546,#11821,#11822) ;
#9473 = AXIS2_PLACEMENT_3D('',#14549,#11824,#11825) ;
#9474 = AXIS2_PLACEMENT_3D('',#14550,#11826,#11827) ;
#9475 = AXIS2_PLACEMENT_3D('',#14551,#11828,#11829) ;
#9476 = AXIS2_PLACEMENT_3D('',#14553,#11831,#11832) ;
#9477 = AXIS2_PLACEMENT_3D('',#14554,#11833,#11834) ;
#9478 = AXIS2_PLACEMENT_3D('',#14556,#11836,#11837) ;
#9479 = AXIS2_PLACEMENT_3D('',#14557,#11838,#11839) ;
#9480 = AXIS2_PLACEMENT_3D('',#14559,#11841,#11842) ;
#9481 = AXIS2_PLACEMENT_3D('',#14560,#11843,#11844) ;
#9482 = AXIS2_PLACEMENT_3D('',#14563,#11846,#11847) ;
#9483 = AXIS2_PLACEMENT_3D('',#14564,#11848,#11849) ;
#9484 = AXIS2_PLACEMENT_3D('',#14565,#11850,#11851) ;
#9485 = AXIS2_PLACEMENT_3D('',#14569,#11853,#11854) ;
#9486 = AXIS2_PLACEMENT_3D('',#14570,#11855,#11856) ;
#9487 = AXIS2_PLACEMENT_3D('',#14571,#11857,#11858) ;
#9488 = AXIS2_PLACEMENT_3D('',#14572,#11859,#11860) ;
#9489 = AXIS2_PLACEMENT_3D('',#14575,#11862,#11863) ;
#9490 = AXIS2_PLACEMENT_3D('',#14576,#11864,#11865) ;
#9491 = AXIS2_PLACEMENT_3D('',#14577,#11866,#11867) ;
#9492 = AXIS2_PLACEMENT_3D('',#14581,#11869,#11870) ;
#9493 = AXIS2_PLACEMENT_3D('',#14582,#11871,#11872) ;
#9494 = AXIS2_PLACEMENT_3D('',#14583,#11873,#11874) ;
#9495 = AXIS2_PLACEMENT_3D('',#14584,#11875,#11876) ;
#9496 = AXIS2_PLACEMENT_3D('',#14587,#11878,#11879) ;
#9497 = AXIS2_PLACEMENT_3D('',#14588,#11880,#11881) ;
#9498 = AXIS2_PLACEMENT_3D('',#14589,#11882,#11883) ;
#9499 = AXIS2_PLACEMENT_3D('',#14591,#11885,#11886) ;
#9500 = AXIS2_PLACEMENT_3D('',#14592,#11887,#11888) ;
#9501 = AXIS2_PLACEMENT_3D('',#14594,#11890,#11891) ;
#9502 = AXIS2_PLACEMENT_3D('',#14595,#11892,#11893) ;
#9503 = AXIS2_PLACEMENT_3D('',#14597,#11895,#11896) ;
#9504 = AXIS2_PLACEMENT_3D('',#14598,#11897,#11898) ;
#9505 = AXIS2_PLACEMENT_3D('',#14601,#11900,#11901) ;
#9506 = AXIS2_PLACEMENT_3D('',#14602,#11902,#11903) ;
#9507 = AXIS2_PLACEMENT_3D('',#14603,#11904,#11905) ;
#9508 = AXIS2_PLACEMENT_3D('',#14607,#11907,#11908) ;
#9509 = AXIS2_PLACEMENT_3D('',#14608,#11909,#11910) ;
#9510 = AXIS2_PLACEMENT_3D('',#14609,#11911,#11912) ;
#9511 = AXIS2_PLACEMENT_3D('',#14610,#11913,#11914) ;
#9512 = AXIS2_PLACEMENT_3D('',#14613,#11916,#11917) ;
#9513 = AXIS2_PLACEMENT_3D('',#14614,#11918,#11919) ;
#9514 = AXIS2_PLACEMENT_3D('',#14615,#11920,#11921) ;
#9515 = AXIS2_PLACEMENT_3D('',#14616,#11922,#11923) ;
#9516 = AXIS2_PLACEMENT_3D('',#14618,#11924,#11925) ;
#9517 = AXIS2_PLACEMENT_3D('',#14621,#11927,#11928) ;
#9518 = AXIS2_PLACEMENT_3D('',#14622,#11929,#11930) ;
#9519 = AXIS2_PLACEMENT_3D('',#14623,#11931,#11932) ;
#9520 = AXIS2_PLACEMENT_3D('',#14632,#11937,#11938) ;
#9521 = AXIS2_PLACEMENT_3D('',#14641,#11943,#11944) ;
#9522 = AXIS2_PLACEMENT_3D('',#14644,#11947,#11948) ;
#9523 = AXIS2_PLACEMENT_3D('',#14646,#11950,#11951) ;
#9524 = AXIS2_PLACEMENT_3D('',#14648,#11953,#11954) ;
#9525 = AXIS2_PLACEMENT_3D('',#14649,#11955,#11956) ;
#9526 = AXIS2_PLACEMENT_3D('',#14650,#11957,#11958) ;
#9527 = AXIS2_PLACEMENT_3D('',#14652,#11959,#11960) ;
#9528 = AXIS2_PLACEMENT_3D('',#14655,#11962,#11963) ;
#9529 = AXIS2_PLACEMENT_3D('',#14656,#11964,#11965) ;
#9530 = AXIS2_PLACEMENT_3D('',#14657,#11966,#11967) ;
#9531 = AXIS2_PLACEMENT_3D('',#14658,#11968,#11969) ;
#9532 = AXIS2_PLACEMENT_3D('',#14660,#11970,#11971) ;
#9533 = AXIS2_PLACEMENT_3D('',#14663,#11973,#11974) ;
#9534 = AXIS2_PLACEMENT_3D('',#14664,#11975,#11976) ;
#9535 = AXIS2_PLACEMENT_3D('',#14665,#11977,#11978) ;
#9536 = AXIS2_PLACEMENT_3D('',#14666,#11979,#11980) ;
#9537 = AXIS2_PLACEMENT_3D('',#14667,#11981,#11982) ;
#9538 = AXIS2_PLACEMENT_3D('',#14669,#11983,#11984) ;
#9539 = AXIS2_PLACEMENT_3D('',#14672,#11986,#11987) ;
#9540 = AXIS2_PLACEMENT_3D('',#14673,#11988,#11989) ;
#9541 = AXIS2_PLACEMENT_3D('',#14674,#11990,#11991) ;
#9542 = AXIS2_PLACEMENT_3D('',#14675,#11992,#11993) ;
#9543 = AXIS2_PLACEMENT_3D('',#14676,#11994,#11995) ;
#9544 = AXIS2_PLACEMENT_3D('',#14678,#11996,#11997) ;
#9545 = AXIS2_PLACEMENT_3D('',#14681,#11999,#12000) ;
#9546 = AXIS2_PLACEMENT_3D('',#14682,#12001,#12002) ;
#9547 = AXIS2_PLACEMENT_3D('',#14683,#12003,#12004) ;
#9548 = AXIS2_PLACEMENT_3D('',#14684,#12005,#12006) ;
#9549 = AXIS2_PLACEMENT_3D('',#14685,#12007,#12008) ;
#9550 = AXIS2_PLACEMENT_3D('',#14688,#12009,#12010) ;
#9551 = AXIS2_PLACEMENT_3D('',#14689,#12011,#12012) ;
#9552 = AXIS2_PLACEMENT_3D('',#14690,#12013,#12014) ;
#9553 = AXIS2_PLACEMENT_3D('',#14693,#12015,#12016) ;
#9554 = AXIS2_PLACEMENT_3D('',#14695,#12017,#12018) ;
#9555 = AXIS2_PLACEMENT_3D('',#14696,#12019,#12020) ;
#9556 = AXIS2_PLACEMENT_3D('',#14697,#12021,#12022) ;
#9557 = AXIS2_PLACEMENT_3D('',#14700,#12023,#12024) ;
#9558 = AXIS2_PLACEMENT_3D('',#14702,#12025,#12026) ;
#9559 = AXIS2_PLACEMENT_3D('',#14704,#12027,#12028) ;
#9560 = AXIS2_PLACEMENT_3D('',#14705,#12029,#12030) ;
#9561 = AXIS2_PLACEMENT_3D('',#14706,#12031,#12032) ;
#9562 = AXIS2_PLACEMENT_3D('',#14709,#12033,#12034) ;
#9563 = AXIS2_PLACEMENT_3D('',#14711,#12035,#12036) ;
#9564 = AXIS2_PLACEMENT_3D('',#14713,#12037,#12038) ;
#9565 = AXIS2_PLACEMENT_3D('',#14714,#12039,#12040) ;
#9566 = AXIS2_PLACEMENT_3D('',#14715,#12041,#12042) ;
#9567 = AXIS2_PLACEMENT_3D('',#14718,#12043,#12044) ;
#9568 = AXIS2_PLACEMENT_3D('',#14720,#12045,#12046) ;
#9569 = AXIS2_PLACEMENT_3D('',#14722,#12047,#12048) ;
#9570 = AXIS2_PLACEMENT_3D('',#14723,#12049,#12050) ;
#9571 = AXIS2_PLACEMENT_3D('',#14724,#12051,#12052) ;
#9572 = AXIS2_PLACEMENT_3D('',#14727,#12053,#12054) ;
#9573 = AXIS2_PLACEMENT_3D('',#14729,#12055,#12056) ;
#9574 = AXIS2_PLACEMENT_3D('',#14730,#12057,#12058) ;
#9575 = AXIS2_PLACEMENT_3D('',#14731,#12059,#12060) ;
#9576 = AXIS2_PLACEMENT_3D('',#14734,#12061,#12062) ;
#9577 = AXIS2_PLACEMENT_3D('',#14735,#12063,#12064) ;
#9578 = AXIS2_PLACEMENT_3D('',#14736,#12065,#12066) ;
#9579 = AXIS2_PLACEMENT_3D('',#14739,#12067,#12068) ;
#9580 = AXIS2_PLACEMENT_3D('',#14740,#12069,#12070) ;
#9581 = AXIS2_PLACEMENT_3D('',#14741,#12071,#12072) ;
#9582 = AXIS2_PLACEMENT_3D('',#14744,#12073,#12074) ;
#9583 = AXIS2_PLACEMENT_3D('',#14745,#12075,#12076) ;
#9584 = AXIS2_PLACEMENT_3D('',#14746,#12077,#12078) ;
#9585 = AXIS2_PLACEMENT_3D('',#14749,#12079,#12080) ;
#9586 = AXIS2_PLACEMENT_3D('',#14751,#12081,#12082) ;
#9587 = AXIS2_PLACEMENT_3D('',#14752,#12083,#12084) ;
#9588 = AXIS2_PLACEMENT_3D('',#14753,#12085,#12086) ;
#9589 = AXIS2_PLACEMENT_3D('',#14756,#12087,#12088) ;
#9590 = AXIS2_PLACEMENT_3D('',#14758,#12089,#12090) ;
#9591 = AXIS2_PLACEMENT_3D('',#14760,#12091,#12092) ;
#9592 = AXIS2_PLACEMENT_3D('',#14761,#12093,#12094) ;
#9593 = AXIS2_PLACEMENT_3D('',#14762,#12095,#12096) ;
#9594 = AXIS2_PLACEMENT_3D('',#14765,#12097,#12098) ;
#9595 = AXIS2_PLACEMENT_3D('',#14767,#12099,#12100) ;
#9596 = AXIS2_PLACEMENT_3D('',#14769,#12101,#12102) ;
#9597 = AXIS2_PLACEMENT_3D('',#14770,#12103,#12104) ;
#9598 = AXIS2_PLACEMENT_3D('',#14771,#12105,#12106) ;
#9599 = AXIS2_PLACEMENT_3D('',#14774,#12107,#12108) ;
#9600 = AXIS2_PLACEMENT_3D('',#14776,#12109,#12110) ;
#9601 = AXIS2_PLACEMENT_3D('',#14778,#12111,#12112) ;
#9602 = AXIS2_PLACEMENT_3D('',#14779,#12113,#12114) ;
#9603 = AXIS2_PLACEMENT_3D('',#14780,#12115,#12116) ;
#9604 = AXIS2_PLACEMENT_3D('',#14783,#12117,#12118) ;
#9605 = AXIS2_PLACEMENT_3D('',#14785,#12119,#12120) ;
#9606 = AXIS2_PLACEMENT_3D('',#14786,#12121,#12122) ;
#9607 = AXIS2_PLACEMENT_3D('',#14787,#12123,#12124) ;
#9608 = AXIS2_PLACEMENT_3D('',#14790,#12125,#12126) ;
#9609 = AXIS2_PLACEMENT_3D('',#14791,#12127,#12128) ;
#9610 = AXIS2_PLACEMENT_3D('',#14792,#12129,#12130) ;
#9611 = AXIS2_PLACEMENT_3D('',#14795,#12131,#12132) ;
#9612 = AXIS2_PLACEMENT_3D('',#14796,#12133,#12134) ;
#9613 = AXIS2_PLACEMENT_3D('',#14797,#12135,#12136) ;
#9614 = AXIS2_PLACEMENT_3D('',#14800,#12137,#12138) ;
#9615 = AXIS2_PLACEMENT_3D('',#14801,#12139,#12140) ;
#9616 = AXIS2_PLACEMENT_3D('',#14802,#12141,#12142) ;
#9617 = AXIS2_PLACEMENT_3D('',#14805,#12143,#12144) ;
#9618 = AXIS2_PLACEMENT_3D('',#14807,#12145,#12146) ;
#9619 = AXIS2_PLACEMENT_3D('',#14808,#12147,#12148) ;
#9620 = AXIS2_PLACEMENT_3D('',#14809,#12149,#12150) ;
#9621 = AXIS2_PLACEMENT_3D('',#14812,#12151,#12152) ;
#9622 = AXIS2_PLACEMENT_3D('',#14814,#12153,#12154) ;
#9623 = AXIS2_PLACEMENT_3D('',#14816,#12155,#12156) ;
#9624 = AXIS2_PLACEMENT_3D('',#14817,#12157,#12158) ;
#9625 = AXIS2_PLACEMENT_3D('',#14818,#12159,#12160) ;
#9626 = AXIS2_PLACEMENT_3D('',#14821,#12161,#12162) ;
#9627 = AXIS2_PLACEMENT_3D('',#14823,#12163,#12164) ;
#9628 = AXIS2_PLACEMENT_3D('',#14825,#12165,#12166) ;
#9629 = AXIS2_PLACEMENT_3D('',#14826,#12167,#12168) ;
#9630 = AXIS2_PLACEMENT_3D('',#14827,#12169,#12170) ;
#9631 = AXIS2_PLACEMENT_3D('',#14830,#12171,#12172) ;
#9632 = AXIS2_PLACEMENT_3D('',#14832,#12173,#12174) ;
#9633 = AXIS2_PLACEMENT_3D('',#14834,#12175,#12176) ;
#9634 = AXIS2_PLACEMENT_3D('',#14835,#12177,#12178) ;
#9635 = AXIS2_PLACEMENT_3D('',#14836,#12179,#12180) ;
#9636 = AXIS2_PLACEMENT_3D('',#14839,#12181,#12182) ;
#9637 = AXIS2_PLACEMENT_3D('',#14841,#12183,#12184) ;
#9638 = AXIS2_PLACEMENT_3D('',#14842,#12185,#12186) ;
#9639 = AXIS2_PLACEMENT_3D('',#14843,#12187,#12188) ;
#9640 = AXIS2_PLACEMENT_3D('',#14846,#12189,#12190) ;
#9641 = AXIS2_PLACEMENT_3D('',#14847,#12191,#12192) ;
#9642 = AXIS2_PLACEMENT_3D('',#14848,#12193,#12194) ;
#9643 = AXIS2_PLACEMENT_3D('',#14851,#12195,#12196) ;
#9644 = AXIS2_PLACEMENT_3D('',#14852,#12197,#12198) ;
#9645 = AXIS2_PLACEMENT_3D('',#14853,#12199,#12200) ;
#9646 = AXIS2_PLACEMENT_3D('',#14856,#12201,#12202) ;
#9647 = AXIS2_PLACEMENT_3D('',#14857,#12203,#12204) ;
#9648 = AXIS2_PLACEMENT_3D('',#14858,#12205,#12206) ;
#9649 = AXIS2_PLACEMENT_3D('',#14861,#12207,#12208) ;
#9650 = AXIS2_PLACEMENT_3D('',#14863,#12209,#12210) ;
#9651 = AXIS2_PLACEMENT_3D('',#14864,#12211,#12212) ;
#9652 = AXIS2_PLACEMENT_3D('',#14865,#12213,#12214) ;
#9653 = AXIS2_PLACEMENT_3D('',#14868,#12215,#12216) ;
#9654 = AXIS2_PLACEMENT_3D('',#14870,#12217,#12218) ;
#9655 = AXIS2_PLACEMENT_3D('',#14872,#12219,#12220) ;
#9656 = AXIS2_PLACEMENT_3D('',#14873,#12221,#12222) ;
#9657 = AXIS2_PLACEMENT_3D('',#14874,#12223,#12224) ;
#9658 = AXIS2_PLACEMENT_3D('',#14877,#12225,#12226) ;
#9659 = AXIS2_PLACEMENT_3D('',#14879,#12227,#12228) ;
#9660 = AXIS2_PLACEMENT_3D('',#14881,#12229,#12230) ;
#9661 = AXIS2_PLACEMENT_3D('',#14882,#12231,#12232) ;
#9662 = AXIS2_PLACEMENT_3D('',#14883,#12233,#12234) ;
#9663 = AXIS2_PLACEMENT_3D('',#14886,#12235,#12236) ;
#9664 = AXIS2_PLACEMENT_3D('',#14888,#12237,#12238) ;
#9665 = AXIS2_PLACEMENT_3D('',#14890,#12239,#12240) ;
#9666 = AXIS2_PLACEMENT_3D('',#14891,#12241,#12242) ;
#9667 = AXIS2_PLACEMENT_3D('',#14892,#12243,#12244) ;
#9668 = AXIS2_PLACEMENT_3D('',#14895,#12245,#12246) ;
#9669 = AXIS2_PLACEMENT_3D('',#14897,#12247,#12248) ;
#9670 = AXIS2_PLACEMENT_3D('',#14898,#12249,#12250) ;
#9671 = AXIS2_PLACEMENT_3D('',#14899,#12251,#12252) ;
#9672 = AXIS2_PLACEMENT_3D('',#14902,#12253,#12254) ;
#9673 = AXIS2_PLACEMENT_3D('',#14903,#12255,#12256) ;
#9674 = AXIS2_PLACEMENT_3D('',#14904,#12257,#12258) ;
#9675 = AXIS2_PLACEMENT_3D('',#14906,#12259,#12260) ;
#9676 = AXIS2_PLACEMENT_3D('',#14910,#12262,#12263) ;
#9677 = AXIS2_PLACEMENT_3D('',#14911,#12264,#12265) ;
#9678 = AXIS2_PLACEMENT_3D('',#14912,#12266,#12267) ;
#9679 = AXIS2_PLACEMENT_3D('',#14913,#12268,#12269) ;
#9680 = AXIS2_PLACEMENT_3D('',#14914,#12270,#12271) ;
#9681 = AXIS2_PLACEMENT_3D('',#14917,#12273,#12274) ;
#9682 = AXIS2_PLACEMENT_3D('',#14918,#12275,#12276) ;
#9683 = AXIS2_PLACEMENT_3D('',#14919,#12277,#12278) ;
#9684 = AXIS2_PLACEMENT_3D('',#14921,#12280,#12281) ;
#9685 = AXIS2_PLACEMENT_3D('',#14922,#12282,#12283) ;
#9686 = AXIS2_PLACEMENT_3D('',#14924,#12285,#12286) ;
#9687 = AXIS2_PLACEMENT_3D('',#14925,#12287,#12288) ;
#9688 = AXIS2_PLACEMENT_3D('',#14927,#12290,#12291) ;
#9689 = AXIS2_PLACEMENT_3D('',#14928,#12292,#12293) ;
#9690 = AXIS2_PLACEMENT_3D('',#14931,#12295,#12296) ;
#9691 = AXIS2_PLACEMENT_3D('',#14932,#12297,#12298) ;
#9692 = AXIS2_PLACEMENT_3D('',#14933,#12299,#12300) ;
#9693 = AXIS2_PLACEMENT_3D('',#14937,#12302,#12303) ;
#9694 = AXIS2_PLACEMENT_3D('',#14938,#12304,#12305) ;
#9695 = AXIS2_PLACEMENT_3D('',#14939,#12306,#12307) ;
#9696 = AXIS2_PLACEMENT_3D('',#14940,#12308,#12309) ;
#9697 = AXIS2_PLACEMENT_3D('',#14943,#12311,#12312) ;
#9698 = AXIS2_PLACEMENT_3D('',#14944,#12313,#12314) ;
#9699 = AXIS2_PLACEMENT_3D('',#14945,#12315,#12316) ;
#9700 = AXIS2_PLACEMENT_3D('',#14949,#12318,#12319) ;
#9701 = AXIS2_PLACEMENT_3D('',#14950,#12320,#12321) ;
#9702 = AXIS2_PLACEMENT_3D('',#14951,#12322,#12323) ;
#9703 = AXIS2_PLACEMENT_3D('',#14952,#12324,#12325) ;
#9704 = AXIS2_PLACEMENT_3D('',#14955,#12327,#12328) ;
#9705 = AXIS2_PLACEMENT_3D('',#14956,#12329,#12330) ;
#9706 = AXIS2_PLACEMENT_3D('',#14957,#12331,#12332) ;
#9707 = AXIS2_PLACEMENT_3D('',#14959,#12334,#12335) ;
#9708 = AXIS2_PLACEMENT_3D('',#14960,#12336,#12337) ;
#9709 = AXIS2_PLACEMENT_3D('',#14962,#12339,#12340) ;
#9710 = AXIS2_PLACEMENT_3D('',#14963,#12341,#12342) ;
#9711 = AXIS2_PLACEMENT_3D('',#14965,#12344,#12345) ;
#9712 = AXIS2_PLACEMENT_3D('',#14966,#12346,#12347) ;
#9713 = AXIS2_PLACEMENT_3D('',#14969,#12349,#12350) ;
#9714 = AXIS2_PLACEMENT_3D('',#14970,#12351,#12352) ;
#9715 = AXIS2_PLACEMENT_3D('',#14971,#12353,#12354) ;
#9716 = AXIS2_PLACEMENT_3D('',#14975,#12356,#12357) ;
#9717 = AXIS2_PLACEMENT_3D('',#14976,#12358,#12359) ;
#9718 = AXIS2_PLACEMENT_3D('',#14977,#12360,#12361) ;
#9719 = AXIS2_PLACEMENT_3D('',#14978,#12362,#12363) ;
#9720 = AXIS2_PLACEMENT_3D('',#14981,#12365,#12366) ;
#9721 = AXIS2_PLACEMENT_3D('',#14982,#12367,#12368) ;
#9722 = AXIS2_PLACEMENT_3D('',#14983,#12369,#12370) ;
#9723 = AXIS2_PLACEMENT_3D('',#14987,#12372,#12373) ;
#9724 = AXIS2_PLACEMENT_3D('',#14988,#12374,#12375) ;
#9725 = AXIS2_PLACEMENT_3D('',#14989,#12376,#12377) ;
#9726 = AXIS2_PLACEMENT_3D('',#14990,#12378,#12379) ;
#9727 = AXIS2_PLACEMENT_3D('',#14993,#12381,#12382) ;
#9728 = AXIS2_PLACEMENT_3D('',#14994,#12383,#12384) ;
#9729 = AXIS2_PLACEMENT_3D('',#14995,#12385,#12386) ;
#9730 = AXIS2_PLACEMENT_3D('',#14997,#12388,#12389) ;
#9731 = AXIS2_PLACEMENT_3D('',#14998,#12390,#12391) ;
#9732 = AXIS2_PLACEMENT_3D('',#15000,#12393,#12394) ;
#9733 = AXIS2_PLACEMENT_3D('',#15001,#12395,#12396) ;
#9734 = AXIS2_PLACEMENT_3D('',#15003,#12398,#12399) ;
#9735 = AXIS2_PLACEMENT_3D('',#15004,#12400,#12401) ;
#9736 = AXIS2_PLACEMENT_3D('',#15007,#12403,#12404) ;
#9737 = AXIS2_PLACEMENT_3D('',#15008,#12405,#12406) ;
#9738 = AXIS2_PLACEMENT_3D('',#15009,#12407,#12408) ;
#9739 = AXIS2_PLACEMENT_3D('',#15013,#12410,#12411) ;
#9740 = AXIS2_PLACEMENT_3D('',#15014,#12412,#12413) ;
#9741 = AXIS2_PLACEMENT_3D('',#15015,#12414,#12415) ;
#9742 = AXIS2_PLACEMENT_3D('',#15016,#12416,#12417) ;
#9743 = AXIS2_PLACEMENT_3D('',#15019,#12419,#12420) ;
#9744 = AXIS2_PLACEMENT_3D('',#15020,#12421,#12422) ;
#9745 = AXIS2_PLACEMENT_3D('',#15021,#12423,#12424) ;
#9746 = AXIS2_PLACEMENT_3D('',#15025,#12426,#12427) ;
#9747 = AXIS2_PLACEMENT_3D('',#15026,#12428,#12429) ;
#9748 = AXIS2_PLACEMENT_3D('',#15027,#12430,#12431) ;
#9749 = AXIS2_PLACEMENT_3D('',#15028,#12432,#12433) ;
#9750 = AXIS2_PLACEMENT_3D('',#15031,#12435,#12436) ;
#9751 = AXIS2_PLACEMENT_3D('',#15032,#12437,#12438) ;
#9752 = AXIS2_PLACEMENT_3D('',#15033,#12439,#12440) ;
#9753 = AXIS2_PLACEMENT_3D('',#15035,#12442,#12443) ;
#9754 = AXIS2_PLACEMENT_3D('',#15036,#12444,#12445) ;
#9755 = AXIS2_PLACEMENT_3D('',#15038,#12447,#12448) ;
#9756 = AXIS2_PLACEMENT_3D('',#15039,#12449,#12450) ;
#9757 = AXIS2_PLACEMENT_3D('',#15041,#12452,#12453) ;
#9758 = AXIS2_PLACEMENT_3D('',#15042,#12454,#12455) ;
#9759 = AXIS2_PLACEMENT_3D('',#15045,#12457,#12458) ;
#9760 = AXIS2_PLACEMENT_3D('',#15046,#12459,#12460) ;
#9761 = AXIS2_PLACEMENT_3D('',#15047,#12461,#12462) ;
#9762 = AXIS2_PLACEMENT_3D('',#15051,#12464,#12465) ;
#9763 = AXIS2_PLACEMENT_3D('',#15052,#12466,#12467) ;
#9764 = AXIS2_PLACEMENT_3D('',#15053,#12468,#12469) ;
#9765 = AXIS2_PLACEMENT_3D('',#15054,#12470,#12471) ;
#9766 = AXIS2_PLACEMENT_3D('',#15057,#12473,#12474) ;
#9767 = AXIS2_PLACEMENT_3D('',#15058,#12475,#12476) ;
#9768 = AXIS2_PLACEMENT_3D('',#15059,#12477,#12478) ;
#9769 = AXIS2_PLACEMENT_3D('',#15060,#12479,#12480) ;
#9770 = AXIS2_PLACEMENT_3D('',#15061,#12481,#12482) ;
#9771 = AXIS2_PLACEMENT_3D('',#15062,#12483,#12484) ;
#9772 = AXIS2_PLACEMENT_3D('',#15063,#12485,#12486) ;
#9773 = AXIS2_PLACEMENT_3D('',#15064,#12487,#12488) ;
#9774 = AXIS2_PLACEMENT_3D('',#15065,#12489,#12490) ;
#9775 = AXIS2_PLACEMENT_3D('',#15066,#12491,#12492) ;
#9776 = AXIS2_PLACEMENT_3D('',#15067,#12493,#12494) ;
#9777 = AXIS2_PLACEMENT_3D('',#15068,#12495,#12496) ;
#9778 = AXIS2_PLACEMENT_3D('',#15069,#12497,#12498) ;
#9779 = AXIS2_PLACEMENT_3D('',#15070,#12499,#12500) ;
#9780 = AXIS2_PLACEMENT_3D('',#15071,#12501,#12502) ;
#9781 = AXIS2_PLACEMENT_3D('',#15072,#12503,#12504) ;
#9782 = AXIS2_PLACEMENT_3D('',#15074,#12505,#12506) ;
#9783 = AXIS2_PLACEMENT_3D('',#15077,#12508,#12509) ;
#9784 = AXIS2_PLACEMENT_3D('',#15078,#12510,#12511) ;
#9785 = AXIS2_PLACEMENT_3D('',#15087,#12516,#12517) ;
#9786 = AXIS2_PLACEMENT_3D('',#15093,#12521,#12522) ;
#9787 = AXIS2_PLACEMENT_3D('',#15099,#12526,#12527) ;
#9788 = AXIS2_PLACEMENT_3D('',#15108,#12532,#12533) ;
#9789 = AXIS2_PLACEMENT_3D('',#15114,#12537,#12538) ;
#9790 = AXIS2_PLACEMENT_3D('',#15120,#12542,#12543) ;
#9791 = AXIS2_PLACEMENT_3D('',#15123,#12546,#12547) ;
#9792 = AXIS2_PLACEMENT_3D('',#15125,#12549,#12550) ;
#9793 = AXIS2_PLACEMENT_3D('',#15127,#12552,#12553) ;
#9794 = AXIS2_PLACEMENT_3D('',#15128,#12554,#12555) ;
#9795 = AXIS2_PLACEMENT_3D('',#15129,#12556,#12557) ;
#9796 = AXIS2_PLACEMENT_3D('',#15138,#12562,#12563) ;
#9797 = AXIS2_PLACEMENT_3D('',#15144,#12567,#12568) ;
#9798 = AXIS2_PLACEMENT_3D('',#15150,#12572,#12573) ;
#9799 = AXIS2_PLACEMENT_3D('',#15153,#12576,#12577) ;
#9800 = AXIS2_PLACEMENT_3D('',#15155,#12578,#12579) ;
#9801 = AXIS2_PLACEMENT_3D('',#15156,#12580,#12581) ;
#9802 = AXIS2_PLACEMENT_3D('',#15159,#12583,#12584) ;
#9803 = AXIS2_PLACEMENT_3D('',#15160,#12585,#12586) ;
#9804 = AXIS2_PLACEMENT_3D('',#15169,#12591,#12592) ;
#9805 = AXIS2_PLACEMENT_3D('',#15178,#12597,#12598) ;
#9806 = AXIS2_PLACEMENT_3D('',#15181,#12601,#12602) ;
#9807 = AXIS2_PLACEMENT_3D('',#15183,#12604,#12605) ;
#9808 = AXIS2_PLACEMENT_3D('',#15185,#12607,#12608) ;
#9809 = AXIS2_PLACEMENT_3D('',#15186,#12609,#12610) ;
#9810 = AXIS2_PLACEMENT_3D('',#15187,#12611,#12612) ;
#9811 = AXIS2_PLACEMENT_3D('',#15190,#12613,#12614) ;
#9812 = AXIS2_PLACEMENT_3D('',#15191,#12615,#12616) ;
#9813 = AXIS2_PLACEMENT_3D('',#15192,#12617,#12618) ;
#9814 = AXIS2_PLACEMENT_3D('',#15193,#12619,#12620) ;
#9815 = AXIS2_PLACEMENT_3D('',#15194,#12621,#12622) ;
#9816 = AXIS2_PLACEMENT_3D('',#15196,#12623,#12624) ;
#9817 = AXIS2_PLACEMENT_3D('',#15198,#12626,#12627) ;
#9818 = AXIS2_PLACEMENT_3D('',#15199,#12628,#12629) ;
#9819 = AXIS2_PLACEMENT_3D('',#15201,#12630,#12631) ;
#9820 = AXIS2_PLACEMENT_3D('',#15204,#12633,#12634) ;
#9821 = AXIS2_PLACEMENT_3D('',#15205,#12635,#12636) ;
#9822 = AXIS2_PLACEMENT_3D('',#15206,#12637,#12638) ;
#9823 = AXIS2_PLACEMENT_3D('',#15207,#12639,#12640) ;
#9824 = AXIS2_PLACEMENT_3D('',#15209,#12641,#12642) ;
#9825 = AXIS2_PLACEMENT_3D('',#15212,#12644,#12645) ;
#9826 = AXIS2_PLACEMENT_3D('',#15213,#12646,#12647) ;
#9827 = AXIS2_PLACEMENT_3D('',#15214,#12648,#12649) ;
#9828 = AXIS2_PLACEMENT_3D('',#15215,#12650,#12651) ;
#9829 = AXIS2_PLACEMENT_3D('',#15216,#12652,#12653) ;
#9830 = AXIS2_PLACEMENT_3D('',#15218,#12654,#12655) ;
#9831 = AXIS2_PLACEMENT_3D('',#15221,#12657,#12658) ;
#9832 = AXIS2_PLACEMENT_3D('',#15222,#12659,#12660) ;
#9833 = AXIS2_PLACEMENT_3D('',#15223,#12661,#12662) ;
#9834 = AXIS2_PLACEMENT_3D('',#15224,#12663,#12664) ;
#9835 = AXIS2_PLACEMENT_3D('',#15226,#12665,#12666) ;
#9836 = AXIS2_PLACEMENT_3D('',#15229,#12668,#12669) ;
#9837 = AXIS2_PLACEMENT_3D('',#15230,#12670,#12671) ;
#9838 = AXIS2_PLACEMENT_3D('',#15231,#12672,#12673) ;
#9839 = AXIS2_PLACEMENT_3D('',#15232,#12674,#12675) ;
#9840 = AXIS2_PLACEMENT_3D('',#15234,#12676,#12677) ;
#9841 = AXIS2_PLACEMENT_3D('',#15237,#12679,#12680) ;
#9842 = AXIS2_PLACEMENT_3D('',#15238,#12681,#12682) ;
#9843 = AXIS2_PLACEMENT_3D('',#15239,#12683,#12684) ;
#9844 = AXIS2_PLACEMENT_3D('',#15240,#12685,#12686) ;
#9845 = AXIS2_PLACEMENT_3D('',#15241,#12687,#12688) ;
#9846 = AXIS2_PLACEMENT_3D('',#15244,#12689,#12690) ;
#9847 = AXIS2_PLACEMENT_3D('',#15255,#12696,#12697) ;
#9848 = AXIS2_PLACEMENT_3D('',#15256,#12698,#12699) ;
#9849 = AXIS2_PLACEMENT_3D('',#15262,#12703,#12704) ;
#9850 = AXIS2_PLACEMENT_3D('',#15268,#12708,#12709) ;
#9851 = AXIS2_PLACEMENT_3D('',#15270,#12710,#12711) ;
#9852 = AXIS2_PLACEMENT_3D('',#15276,#12715,#12716) ;
#9853 = AXIS2_PLACEMENT_3D('',#15277,#12717,#12718) ;
#9854 = AXIS2_PLACEMENT_3D('',#15287,#12724,#12725) ;
#9855 = AXIS2_PLACEMENT_3D('',#15291,#12728,#12729) ;
#9856 = AXIS2_PLACEMENT_3D('',#15295,#12732,#12733) ;
#9857 = AXIS2_PLACEMENT_3D('',#15297,#12734,#12735) ;
#9858 = AXIS2_PLACEMENT_3D('',#15301,#12738,#12739) ;
#9859 = AXIS2_PLACEMENT_3D('',#15302,#12740,#12741) ;
#9860 = AXIS2_PLACEMENT_3D('',#15308,#12745,#12746) ;
#9861 = AXIS2_PLACEMENT_3D('',#15311,#12749,#12750) ;
#9862 = AXIS2_PLACEMENT_3D('',#15312,#12751,#12752) ;
#9863 = AXIS2_PLACEMENT_3D('',#15313,#12753,#12754) ;
#9864 = AXIS2_PLACEMENT_3D('',#15314,#12755,#12756) ;
#9865 = AXIS2_PLACEMENT_3D('',#15316,#12757,#12758) ;
#9866 = AXIS2_PLACEMENT_3D('',#15319,#12760,#12761) ;
#9867 = AXIS2_PLACEMENT_3D('',#15320,#12762,#12763) ;
#9868 = AXIS2_PLACEMENT_3D('',#15321,#12764,#12765) ;
#9869 = AXIS2_PLACEMENT_3D('',#15322,#12766,#12767) ;
#9870 = AXIS2_PLACEMENT_3D('',#15324,#12768,#12769) ;
#9871 = AXIS2_PLACEMENT_3D('',#15327,#12771,#12772) ;
#9872 = AXIS2_PLACEMENT_3D('',#15328,#12773,#12774) ;
#9873 = AXIS2_PLACEMENT_3D('',#15329,#12775,#12776) ;
#9874 = AXIS2_PLACEMENT_3D('',#15330,#12777,#12778) ;
#9875 = AXIS2_PLACEMENT_3D('',#15332,#12779,#12780) ;
#9876 = AXIS2_PLACEMENT_3D('',#15335,#12782,#12783) ;
#9877 = AXIS2_PLACEMENT_3D('',#15336,#12784,#12785) ;
#9878 = AXIS2_PLACEMENT_3D('',#15337,#12786,#12787) ;
#9879 = AXIS2_PLACEMENT_3D('',#15338,#12788,#12789) ;
#9880 = AXIS2_PLACEMENT_3D('',#15339,#12790,#12791) ;
#9881 = AXIS2_PLACEMENT_3D('',#15341,#12792,#12793) ;
#9882 = AXIS2_PLACEMENT_3D('',#15344,#12795,#12796) ;
#9883 = AXIS2_PLACEMENT_3D('',#15345,#12797,#12798) ;
#9884 = AXIS2_PLACEMENT_3D('',#15346,#12799,#12800) ;
#9885 = AXIS2_PLACEMENT_3D('',#15347,#12801,#12802) ;
#9886 = AXIS2_PLACEMENT_3D('',#15348,#12803,#12804) ;
#9887 = AXIS2_PLACEMENT_3D('',#15349,#12805,#12806) ;
#9888 = AXIS2_PLACEMENT_3D('',#15350,#12807,#12808) ;
#9889 = AXIS2_PLACEMENT_3D('',#15351,#12809,#12810) ;
#9890 = AXIS2_PLACEMENT_3D('',#15352,#12811,#12812) ;
#9891 = AXIS2_PLACEMENT_3D('',#15353,#12813,#12814) ;
#9892 = AXIS2_PLACEMENT_3D('',#15354,#12815,#12816) ;
#9893 = AXIS2_PLACEMENT_3D('',#15355,#12817,#12818) ;
#9894 = AXIS2_PLACEMENT_3D('',#15356,#12819,#12820) ;
#9895 = AXIS2_PLACEMENT_3D('',#15357,#12821,#12822) ;
#9896 = AXIS2_PLACEMENT_3D('',#15358,#12823,#12824) ;
#9897 = AXIS2_PLACEMENT_3D('',#15360,#12825,#12826) ;
#9898 = AXIS2_PLACEMENT_3D('',#15363,#12828,#12829) ;
#9899 = AXIS2_PLACEMENT_3D('',#15364,#12830,#12831) ;
#9900 = AXIS2_PLACEMENT_3D('',#15365,#12832,#12833) ;
#9901 = AXIS2_PLACEMENT_3D('',#15367,#12834,#12835) ;
#9902 = AXIS2_PLACEMENT_3D('',#15370,#12837,#12838) ;
#9903 = AXIS2_PLACEMENT_3D('',#15371,#12839,#12840) ;
#9904 = AXIS2_PLACEMENT_3D('',#15372,#12841,#12842) ;
#9905 = AXIS2_PLACEMENT_3D('',#15373,#12843,#12844) ;
#9906 = AXIS2_PLACEMENT_3D('',#15374,#12845,#12846) ;
#9907 = AXIS2_PLACEMENT_3D('',#15376,#12847,#12848) ;
#9908 = AXIS2_PLACEMENT_3D('',#15379,#12850,#12851) ;
#9909 = AXIS2_PLACEMENT_3D('',#15380,#12852,#12853) ;
#9910 = AXIS2_PLACEMENT_3D('',#15381,#12854,#12855) ;
#9911 = AXIS2_PLACEMENT_3D('',#15383,#12856,#12857) ;
#9912 = AXIS2_PLACEMENT_3D('',#15386,#12859,#12860) ;
#9913 = AXIS2_PLACEMENT_3D('',#15387,#12861,#12862) ;
#9914 = AXIS2_PLACEMENT_3D('',#15388,#12863,#12864) ;
#9915 = AXIS2_PLACEMENT_3D('',#15389,#12865,#12866) ;
#9916 = AXIS2_PLACEMENT_3D('',#15390,#12867,#12868) ;
#9917 = AXIS2_PLACEMENT_3D('',#15391,#12869,#12870) ;
#9918 = AXIS2_PLACEMENT_3D('',#15392,#12871,#12872) ;
#9919 = AXIS2_PLACEMENT_3D('',#15393,#12873,#12874) ;
#9920 = AXIS2_PLACEMENT_3D('',#15394,#12875,#12876) ;
#9921 = AXIS2_PLACEMENT_3D('',#15395,#12877,#12878) ;
#9922 = AXIS2_PLACEMENT_3D('',#15396,#12879,#12880) ;
#9923 = AXIS2_PLACEMENT_3D('',#15397,#12881,#12882) ;
#9924 = AXIS2_PLACEMENT_3D('',#15398,#12883,#12884) ;
#9925 = DIRECTION('axis',(0.,0.,1.)) ;
#9926 = DIRECTION('refdir',(1.,0.,0.)) ;
#9927 = DIRECTION('axis',(0.,0.,1.)) ;
#9928 = DIRECTION('refdir',(1.,0.,0.)) ;
#9929 = DIRECTION('axis',(0.,0.,1.)) ;
#9930 = DIRECTION('refdir',(1.,0.,0.)) ;
#9931 = DIRECTION('center_axis',(0.,0.,1.)) ;
#9932 = DIRECTION('ref_axis',(1.,0.,0.)) ;
#9933 = DIRECTION('',(0.,-1.,0.)) ;
#9934 = DIRECTION('',(1.,0.,0.)) ;
#9935 = DIRECTION('',(0.,1.,0.)) ;
#9936 = DIRECTION('',(-1.,0.,0.)) ;
#9937 = DIRECTION('center_axis',(0.,1.,0.)) ;
#9938 = DIRECTION('ref_axis',(0.,0.,1.)) ;
#9939 = DIRECTION('',(0.,0.,-1.)) ;
#9940 = DIRECTION('',(-1.,0.,0.)) ;
#9941 = DIRECTION('',(0.,0.,-1.)) ;
#9942 = DIRECTION('',(-1.,0.,0.)) ;
#9943 = DIRECTION('',(0.,0.,-1.)) ;
#9944 = DIRECTION('center_axis',(1.,0.,0.)) ;
#9945 = DIRECTION('ref_axis',(0.,0.,-1.)) ;
#9946 = DIRECTION('',(0.,0.,-1.)) ;
#9947 = DIRECTION('',(0.,1.,0.)) ;
#9948 = DIRECTION('',(0.,0.,-1.)) ;
#9949 = DIRECTION('',(0.,1.,0.)) ;
#9950 = DIRECTION('center_axis',(0.,-1.,0.)) ;
#9951 = DIRECTION('ref_axis',(0.,0.,-1.)) ;
#9952 = DIRECTION('',(0.,0.,-1.)) ;
#9953 = DIRECTION('',(1.,0.,0.)) ;
#9954 = DIRECTION('center_axis',(-1.,0.,0.)) ;
#9955 = DIRECTION('ref_axis',(0.,0.,1.)) ;
#9956 = DIRECTION('',(0.,-1.,0.)) ;
#9957 = DIRECTION('center_axis',(0.,0.,1.)) ;
#9958 = DIRECTION('ref_axis',(1.,0.,0.)) ;
#9959 = DIRECTION('',(0.,-1.,0.)) ;
#9960 = DIRECTION('',(1.,0.,0.)) ;
#9961 = DIRECTION('center_axis',(0.,0.,-1.)) ;
#9962 = DIRECTION('ref_axis',(1.,0.,0.)) ;
#9963 = DIRECTION('center_axis',(0.,0.,-1.)) ;
#9964 = DIRECTION('ref_axis',(1.,0.,0.)) ;
#9965 = DIRECTION('',(-1.,0.,0.)) ;
#9966 = DIRECTION('',(0.,1.,0.)) ;
#9967 = DIRECTION('',(1.,0.,0.)) ;
#9968 = DIRECTION('',(0.,-1.,0.)) ;
#9969 = DIRECTION('',(-1.,0.,0.)) ;
#9970 = DIRECTION('',(0.,1.,0.)) ;
#9971 = DIRECTION('',(1.,0.,0.)) ;
#9972 = DIRECTION('',(0.,-1.,0.)) ;
#9973 = DIRECTION('center_axis',(0.,0.,-1.)) ;
#9974 = DIRECTION('ref_axis',(1.,0.,0.)) ;
#9975 = DIRECTION('center_axis',(0.,0.,-1.)) ;
#9976 = DIRECTION('ref_axis',(1.,0.,0.)) ;
#9977 = DIRECTION('center_axis',(0.,0.,1.)) ;
#9978 = DIRECTION('ref_axis',(1.,0.,0.)) ;
#9979 = DIRECTION('center_axis',(0.,0.,1.)) ;
#9980 = DIRECTION('ref_axis',(1.,0.,0.)) ;
#9981 = DIRECTION('',(0.,0.,1.)) ;
#9982 = DIRECTION('center_axis',(0.,0.,1.)) ;
#9983 = DIRECTION('ref_axis',(1.,0.,0.)) ;
#9984 = DIRECTION('center_axis',(0.,0.,1.)) ;
#9985 = DIRECTION('ref_axis',(1.,0.,0.)) ;
#9986 = DIRECTION('center_axis',(0.,0.,1.)) ;
#9987 = DIRECTION('ref_axis',(1.,0.,0.)) ;
#9988 = DIRECTION('center_axis',(0.,0.,1.)) ;
#9989 = DIRECTION('ref_axis',(1.,0.,0.)) ;
#9990 = DIRECTION('',(0.,0.,1.)) ;
#9991 = DIRECTION('center_axis',(0.,0.,1.)) ;
#9992 = DIRECTION('ref_axis',(1.,0.,0.)) ;
#9993 = DIRECTION('center_axis',(0.,0.,1.)) ;
#9994 = DIRECTION('ref_axis',(1.,0.,0.)) ;
#9995 = DIRECTION('center_axis',(0.,0.,1.)) ;
#9996 = DIRECTION('ref_axis',(1.,0.,0.)) ;
#9997 = DIRECTION('center_axis',(0.,0.,1.)) ;
#9998 = DIRECTION('ref_axis',(1.,0.,0.)) ;
#9999 = DIRECTION('',(0.,0.,1.)) ;
#10000 = DIRECTION('center_axis',(0.,0.,-1.)) ;
#10001 = DIRECTION('ref_axis',(1.,0.,0.)) ;
#10002 = DIRECTION('center_axis',(0.,0.,1.)) ;
#10003 = DIRECTION('ref_axis',(1.,0.,0.)) ;
#10004 = DIRECTION('',(0.,1.,0.)) ;
#10005 = DIRECTION('',(1.,0.,0.)) ;
#10006 = DIRECTION('',(0.,-1.,0.)) ;
#10007 = DIRECTION('',(1.,0.,0.)) ;
#10008 = DIRECTION('center_axis',(0.,1.,0.)) ;
#10009 = DIRECTION('ref_axis',(0.,0.,1.)) ;
#10010 = DIRECTION('',(0.,0.,-1.)) ;
#10011 = DIRECTION('',(-1.,0.,0.)) ;
#10012 = DIRECTION('',(0.,0.,-1.)) ;
#10013 = DIRECTION('center_axis',(1.,0.,0.)) ;
#10014 = DIRECTION('ref_axis',(0.,0.,-1.)) ;
#10015 = DIRECTION('',(0.,0.,1.)) ;
#10016 = DIRECTION('',(0.,1.,0.)) ;
#10017 = DIRECTION('center_axis',(-1.,0.,0.)) ;
#10018 = DIRECTION('ref_axis',(0.,0.,1.)) ;
#10019 = DIRECTION('',(0.,-1.,0.)) ;
#10020 = DIRECTION('',(0.,0.,-1.)) ;
#10021 = DIRECTION('center_axis',(0.,1.,0.)) ;
#10022 = DIRECTION('ref_axis',(0.,0.,1.)) ;
#10023 = DIRECTION('',(-1.,0.,0.)) ;
#10024 = DIRECTION('',(0.,0.,-1.)) ;
#10025 = DIRECTION('',(1.,0.,0.)) ;
#10026 = DIRECTION('',(0.,0.,-1.)) ;
#10027 = DIRECTION('',(-1.,0.,0.)) ;
#10028 = DIRECTION('center_axis',(0.,0.,1.)) ;
#10029 = DIRECTION('ref_axis',(1.,0.,0.)) ;
#10030 = DIRECTION('center_axis',(0.,0.,1.)) ;
#10031 = DIRECTION('ref_axis',(1.,0.,0.)) ;
#10032 = DIRECTION('',(0.,0.,1.)) ;
#10033 = DIRECTION('center_axis',(0.,0.,-1.)) ;
#10034 = DIRECTION('ref_axis',(1.,0.,0.)) ;
#10035 = DIRECTION('center_axis',(0.,0.,1.)) ;
#10036 = DIRECTION('ref_axis',(1.,0.,0.)) ;
#10037 = DIRECTION('',(0.,1.,0.)) ;
#10038 = DIRECTION('',(-1.,0.,0.)) ;
#10039 = DIRECTION('',(0.,-1.,0.)) ;
#10040 = DIRECTION('',(-1.,0.,0.)) ;
#10041 = DIRECTION('center_axis',(1.,0.,0.)) ;
#10042 = DIRECTION('ref_axis',(0.,0.,-1.)) ;
#10043 = DIRECTION('',(0.,0.,-1.)) ;
#10044 = DIRECTION('',(0.,1.,0.)) ;
#10045 = DIRECTION('',(0.,0.,-1.)) ;
#10046 = DIRECTION('center_axis',(0.,-1.,0.)) ;
#10047 = DIRECTION('ref_axis',(0.,0.,-1.)) ;
#10048 = DIRECTION('',(0.,0.,-1.)) ;
#10049 = DIRECTION('',(1.,0.,0.)) ;
#10050 = DIRECTION('center_axis',(-1.,0.,0.)) ;
#10051 = DIRECTION('ref_axis',(0.,0.,1.)) ;
#10052 = DIRECTION('',(0.,0.,1.)) ;
#10053 = DIRECTION('',(0.,-1.,0.)) ;
#10054 = DIRECTION('center_axis',(0.,-1.,0.)) ;
#10055 = DIRECTION('ref_axis',(0.,0.,-1.)) ;
#10056 = DIRECTION('',(1.,0.,0.)) ;
#10057 = DIRECTION('',(0.,0.,-1.)) ;
#10058 = DIRECTION('',(-1.,0.,0.)) ;
#10059 = DIRECTION('',(0.,0.,-1.)) ;
#10060 = DIRECTION('',(1.,0.,0.)) ;
#10061 = DIRECTION('center_axis',(0.,0.,1.)) ;
#10062 = DIRECTION('ref_axis',(1.,0.,0.)) ;
#10063 = DIRECTION('center_axis',(0.,0.,1.)) ;
#10064 = DIRECTION('ref_axis',(1.,0.,0.)) ;
#10065 = DIRECTION('',(0.,0.,1.)) ;
#10066 = DIRECTION('center_axis',(0.,0.,-1.)) ;
#10067 = DIRECTION('ref_axis',(1.,0.,0.)) ;
#10068 = DIRECTION('center_axis',(0.,0.,1.)) ;
#10069 = DIRECTION('ref_axis',(1.,0.,0.)) ;
#10070 = DIRECTION('center_axis',(0.,0.,1.)) ;
#10071 = DIRECTION('ref_axis',(1.,0.,0.)) ;
#10072 = DIRECTION('',(0.,0.,-1.)) ;
#10073 = DIRECTION('center_axis',(0.,0.,1.)) ;
#10074 = DIRECTION('ref_axis',(1.,0.,0.)) ;
#10075 = DIRECTION('center_axis',(0.,0.,1.)) ;
#10076 = DIRECTION('ref_axis',(1.,0.,0.)) ;
#10077 = DIRECTION('center_axis',(0.,0.,1.)) ;
#10078 = DIRECTION('ref_axis',(1.,0.,0.)) ;
#10079 = DIRECTION('center_axis',(0.,0.,1.)) ;
#10080 = DIRECTION('ref_axis',(1.,0.,0.)) ;
#10081 = DIRECTION('',(0.,0.,1.)) ;
#10082 = DIRECTION('center_axis',(0.,0.,-1.)) ;
#10083 = DIRECTION('ref_axis',(1.,0.,0.)) ;
#10084 = DIRECTION('center_axis',(0.,0.,1.)) ;
#10085 = DIRECTION('ref_axis',(1.,0.,0.)) ;
#10086 = DIRECTION('center_axis',(0.,0.,1.)) ;
#10087 = DIRECTION('ref_axis',(1.,0.,0.)) ;
#10088 = DIRECTION('',(0.,0.,-1.)) ;
#10089 = DIRECTION('center_axis',(0.,0.,1.)) ;
#10090 = DIRECTION('ref_axis',(1.,0.,0.)) ;
#10091 = DIRECTION('center_axis',(0.,0.,1.)) ;
#10092 = DIRECTION('ref_axis',(1.,0.,0.)) ;
#10093 = DIRECTION('center_axis',(0.,0.,1.)) ;
#10094 = DIRECTION('ref_axis',(1.,0.,0.)) ;
#10095 = DIRECTION('',(0.,0.,1.)) ;
#10096 = DIRECTION('center_axis',(0.,0.,-1.)) ;
#10097 = DIRECTION('ref_axis',(1.,0.,0.)) ;
#10098 = DIRECTION('center_axis',(0.,0.,1.)) ;
#10099 = DIRECTION('ref_axis',(1.,0.,0.)) ;
#10100 = DIRECTION('center_axis',(0.,0.,1.)) ;
#10101 = DIRECTION('ref_axis',(1.,0.,0.)) ;
#10102 = DIRECTION('',(0.,0.,-1.)) ;
#10103 = DIRECTION('center_axis',(0.,0.,1.)) ;
#10104 = DIRECTION('ref_axis',(1.,0.,0.)) ;
#10105 = DIRECTION('center_axis',(0.,0.,1.)) ;
#10106 = DIRECTION('ref_axis',(1.,0.,0.)) ;
#10107 = DIRECTION('center_axis',(0.,1.,0.)) ;
#10108 = DIRECTION('ref_axis',(1.,0.,0.)) ;
#10109 = DIRECTION('center_axis',(0.,1.,0.)) ;
#10110 = DIRECTION('ref_axis',(1.,0.,0.)) ;
#10111 = DIRECTION('',(0.,1.,0.)) ;
#10112 = DIRECTION('center_axis',(0.,-1.,0.)) ;
#10113 = DIRECTION('ref_axis',(1.,0.,0.)) ;
#10114 = DIRECTION('center_axis',(0.,1.,0.)) ;
#10115 = DIRECTION('ref_axis',(1.,0.,0.)) ;
#10116 = DIRECTION('center_axis',(0.,1.,0.)) ;
#10117 = DIRECTION('ref_axis',(1.,0.,0.)) ;
#10118 = DIRECTION('',(0.,1.,0.)) ;
#10119 = DIRECTION('center_axis',(0.,-1.,0.)) ;
#10120 = DIRECTION('ref_axis',(1.,0.,0.)) ;
#10121 = DIRECTION('center_axis',(0.,0.,1.)) ;
#10122 = DIRECTION('ref_axis',(1.,0.,0.)) ;
#10123 = DIRECTION('',(0.,1.,0.)) ;
#10124 = DIRECTION('',(-1.,0.,0.)) ;
#10125 = DIRECTION('',(0.,-1.,0.)) ;
#10126 = DIRECTION('',(1.,0.,0.)) ;
#10127 = DIRECTION('center_axis',(0.,1.,0.)) ;
#10128 = DIRECTION('ref_axis',(0.,0.,1.)) ;
#10129 = DIRECTION('',(0.,0.,-1.)) ;
#10130 = DIRECTION('',(0.,0.,-1.)) ;
#10131 = DIRECTION('center_axis',(1.,0.,0.)) ;
#10132 = DIRECTION('ref_axis',(0.,0.,-1.)) ;
#10133 = DIRECTION('',(0.,0.,-1.)) ;
#10134 = DIRECTION('center_axis',(0.,-1.,0.)) ;
#10135 = DIRECTION('ref_axis',(0.,0.,-1.)) ;
#10136 = DIRECTION('',(0.,0.,-1.)) ;
#10137 = DIRECTION('center_axis',(-1.,0.,0.)) ;
#10138 = DIRECTION('ref_axis',(0.,0.,1.)) ;
#10139 = DIRECTION('center_axis',(0.,0.,1.)) ;
#10140 = DIRECTION('ref_axis',(1.,0.,0.)) ;
#10141 = DIRECTION('',(0.,1.,0.)) ;
#10142 = DIRECTION('',(-1.,0.,0.)) ;
#10143 = DIRECTION('',(0.,-1.,0.)) ;
#10144 = DIRECTION('',(1.,0.,0.)) ;
#10145 = DIRECTION('center_axis',(0.,1.,0.)) ;
#10146 = DIRECTION('ref_axis',(0.,0.,1.)) ;
#10147 = DIRECTION('',(0.,0.,-1.)) ;
#10148 = DIRECTION('',(0.,0.,-1.)) ;
#10149 = DIRECTION('center_axis',(1.,0.,0.)) ;
#10150 = DIRECTION('ref_axis',(0.,0.,-1.)) ;
#10151 = DIRECTION('',(0.,0.,-1.)) ;
#10152 = DIRECTION('center_axis',(0.,-1.,0.)) ;
#10153 = DIRECTION('ref_axis',(0.,0.,-1.)) ;
#10154 = DIRECTION('',(0.,0.,-1.)) ;
#10155 = DIRECTION('center_axis',(-1.,0.,0.)) ;
#10156 = DIRECTION('ref_axis',(0.,0.,1.)) ;
#10157 = DIRECTION('center_axis',(0.,0.,1.)) ;
#10158 = DIRECTION('ref_axis',(1.,0.,0.)) ;
#10159 = DIRECTION('center_axis',(0.,0.,1.)) ;
#10160 = DIRECTION('ref_axis',(1.,0.,0.)) ;
#10161 = DIRECTION('',(0.,0.,1.)) ;
#10162 = DIRECTION('center_axis',(0.,-1.,0.)) ;
#10163 = DIRECTION('ref_axis',(0.,0.,-1.)) ;
#10164 = DIRECTION('',(1.,0.,0.)) ;
#10165 = DIRECTION('',(0.,0.,-1.)) ;
#10166 = DIRECTION('center_axis',(-1.,0.,0.)) ;
#10167 = DIRECTION('ref_axis',(0.,0.,1.)) ;
#10168 = DIRECTION('',(0.,-1.,0.)) ;
#10169 = DIRECTION('center_axis',(0.,0.,1.)) ;
#10170 = DIRECTION('ref_axis',(1.,0.,0.)) ;
#10171 = DIRECTION('center_axis',(0.,0.,1.)) ;
#10172 = DIRECTION('ref_axis',(1.,0.,0.)) ;
#10173 = DIRECTION('',(0.,1.,0.)) ;
#10174 = DIRECTION('',(0.,-1.,0.)) ;
#10175 = DIRECTION('center_axis',(0.,0.,1.)) ;
#10176 = DIRECTION('ref_axis',(1.,0.,0.)) ;
#10177 = DIRECTION('',(0.,-1.,0.)) ;
#10178 = DIRECTION('',(0.,1.,0.)) ;
#10179 = DIRECTION('center_axis',(1.,0.,0.)) ;
#10180 = DIRECTION('ref_axis',(0.,0.,-1.)) ;
#10181 = DIRECTION('center_axis',(-1.,0.,0.)) ;
#10182 = DIRECTION('ref_axis',(0.,0.,1.)) ;
#10183 = DIRECTION('axis',(0.,0.,1.)) ;
#10184 = DIRECTION('refdir',(1.,0.,0.)) ;
#10185 = DIRECTION('center_axis',(0.,0.,1.)) ;
#10186 = DIRECTION('ref_axis',(1.,0.,0.)) ;
#10187 = DIRECTION('',(0.,0.,-1.)) ;
#10188 = DIRECTION('center_axis',(0.,0.,1.)) ;
#10189 = DIRECTION('ref_axis',(1.,0.,0.)) ;
#10190 = DIRECTION('',(0.,0.,1.)) ;
#10191 = DIRECTION('center_axis',(0.,0.,1.)) ;
#10192 = DIRECTION('ref_axis',(1.,0.,0.)) ;
#10193 = DIRECTION('center_axis',(0.,0.,1.)) ;
#10194 = DIRECTION('ref_axis',(1.,0.,0.)) ;
#10195 = DIRECTION('',(0.,1.,0.)) ;
#10196 = DIRECTION('center_axis',(0.,0.,1.)) ;
#10197 = DIRECTION('ref_axis',(1.,0.,0.)) ;
#10198 = DIRECTION('',(-1.,0.,0.)) ;
#10199 = DIRECTION('center_axis',(0.,0.,-1.)) ;
#10200 = DIRECTION('ref_axis',(1.,0.,0.)) ;
#10201 = DIRECTION('center_axis',(0.,0.,1.)) ;
#10202 = DIRECTION('ref_axis',(-0.794686467668033,-0.60702011342731,0.)) ;
#10203 = DIRECTION('',(0.,0.,1.)) ;
#10204 = DIRECTION('center_axis',(0.,0.,1.)) ;
#10205 = DIRECTION('ref_axis',(1.,0.,0.)) ;
#10206 = DIRECTION('',(0.,0.,-1.)) ;
#10207 = DIRECTION('center_axis',(-1.,0.,0.)) ;
#10208 = DIRECTION('ref_axis',(0.,0.,1.)) ;
#10209 = DIRECTION('',(0.,-1.,0.)) ;
#10210 = DIRECTION('',(0.,0.,-1.)) ;
#10211 = DIRECTION('',(0.,1.,0.)) ;
#10212 = DIRECTION('',(0.,0.,-1.)) ;
#10213 = DIRECTION('',(0.,-1.,0.)) ;
#10214 = DIRECTION('center_axis',(-1.,0.,0.)) ;
#10215 = DIRECTION('ref_axis',(0.,0.,-1.)) ;
#10216 = DIRECTION('center_axis',(0.,0.,1.)) ;
#10217 = DIRECTION('ref_axis',(1.,0.,0.)) ;
#10218 = DIRECTION('',(1.,0.,0.)) ;
#10219 = DIRECTION('center_axis',(0.,0.,1.)) ;
#10220 = DIRECTION('ref_axis',(1.,0.,0.)) ;
#10221 = DIRECTION('',(0.,0.,1.)) ;
#10222 = DIRECTION('center_axis',(0.,0.,-1.)) ;
#10223 = DIRECTION('ref_axis',(1.,0.,0.)) ;
#10224 = DIRECTION('center_axis',(0.,0.,1.)) ;
#10225 = DIRECTION('ref_axis',(1.,0.,0.)) ;
#10226 = DIRECTION('',(0.,0.,1.)) ;
#10227 = DIRECTION('center_axis',(0.,0.,1.)) ;
#10228 = DIRECTION('ref_axis',(1.,0.,0.)) ;
#10229 = DIRECTION('',(0.,0.,-1.)) ;
#10230 = DIRECTION('center_axis',(0.,0.,1.)) ;
#10231 = DIRECTION('ref_axis',(1.,0.,0.)) ;
#10232 = DIRECTION('center_axis',(0.,0.,1.)) ;
#10233 = DIRECTION('ref_axis',(1.,0.,0.)) ;
#10234 = DIRECTION('',(0.,0.,-1.)) ;
#10235 = DIRECTION('center_axis',(0.,0.,1.)) ;
#10236 = DIRECTION('ref_axis',(1.,0.,0.)) ;
#10237 = DIRECTION('',(0.,0.,1.)) ;
#10238 = DIRECTION('center_axis',(0.,0.,1.)) ;
#10239 = DIRECTION('ref_axis',(1.,0.,0.)) ;
#10240 = DIRECTION('center_axis',(0.,0.,1.)) ;
#10241 = DIRECTION('ref_axis',(1.,0.,0.)) ;
#10242 = DIRECTION('',(0.,-1.,0.)) ;
#10243 = DIRECTION('',(-1.,0.,0.)) ;
#10244 = DIRECTION('center_axis',(0.,0.,-1.)) ;
#10245 = DIRECTION('ref_axis',(1.,0.,0.)) ;
#10246 = DIRECTION('center_axis',(0.,-1.,0.)) ;
#10247 = DIRECTION('ref_axis',(0.,0.,-1.)) ;
#10248 = DIRECTION('',(1.,0.,0.)) ;
#10249 = DIRECTION('',(1.,0.,0.)) ;
#10250 = DIRECTION('',(0.,0.,-1.)) ;
#10251 = DIRECTION('',(-1.,0.,0.)) ;
#10252 = DIRECTION('center_axis',(0.,0.,1.)) ;
#10253 = DIRECTION('ref_axis',(1.,0.,0.)) ;
#10254 = DIRECTION('',(0.,1.,0.)) ;
#10255 = DIRECTION('center_axis',(0.,0.,1.)) ;
#10256 = DIRECTION('ref_axis',(1.,0.,0.)) ;
#10257 = DIRECTION('',(-1.,0.,0.)) ;
#10258 = DIRECTION('',(0.,1.,0.)) ;
#10259 = DIRECTION('center_axis',(0.,0.,1.)) ;
#10260 = DIRECTION('ref_axis',(1.,0.,0.)) ;
#10261 = DIRECTION('',(0.,0.,1.)) ;
#10262 = DIRECTION('center_axis',(0.,0.,-1.)) ;
#10263 = DIRECTION('ref_axis',(1.,0.,0.)) ;
#10264 = DIRECTION('center_axis',(1.,0.,0.)) ;
#10265 = DIRECTION('ref_axis',(0.,0.,-1.)) ;
#10266 = DIRECTION('center_axis',(1.,0.,0.)) ;
#10267 = DIRECTION('ref_axis',(0.,0.,-1.)) ;
#10268 = DIRECTION('',(1.,0.,0.)) ;
#10269 = DIRECTION('center_axis',(0.,0.,1.)) ;
#10270 = DIRECTION('ref_axis',(1.,0.,0.)) ;
#10271 = DIRECTION('',(0.,-1.,0.)) ;
#10272 = DIRECTION('',(1.,0.,0.)) ;
#10273 = DIRECTION('center_axis',(0.,1.,0.)) ;
#10274 = DIRECTION('ref_axis',(0.,0.,1.)) ;
#10275 = DIRECTION('',(0.,0.,-1.)) ;
#10276 = DIRECTION('center_axis',(1.,0.,0.)) ;
#10277 = DIRECTION('ref_axis',(0.,0.,-1.)) ;
#10278 = DIRECTION('',(0.,0.,1.)) ;
#10279 = DIRECTION('',(1.,0.,0.)) ;
#10280 = DIRECTION('',(0.,0.,1.)) ;
#10281 = DIRECTION('',(1.,0.,0.)) ;
#10282 = DIRECTION('axis',(0.,0.,1.)) ;
#10283 = DIRECTION('refdir',(1.,0.,0.)) ;
#10284 = DIRECTION('axis',(0.,0.,1.)) ;
#10285 = DIRECTION('refdir',(1.,0.,0.)) ;
#10286 = DIRECTION('center_axis',(0.,0.,1.)) ;
#10287 = DIRECTION('ref_axis',(1.,0.,0.)) ;
#10288 = DIRECTION('center_axis',(0.,0.,1.)) ;
#10289 = DIRECTION('ref_axis',(1.,0.,0.)) ;
#10290 = DIRECTION('',(0.,0.,1.)) ;
#10291 = DIRECTION('center_axis',(0.,0.,1.)) ;
#10292 = DIRECTION('ref_axis',(1.,0.,0.)) ;
#10293 = DIRECTION('center_axis',(0.,0.,1.)) ;
#10294 = DIRECTION('ref_axis',(1.,0.,0.)) ;
#10295 = DIRECTION('center_axis',(0.,-1.,0.)) ;
#10296 = DIRECTION('ref_axis',(0.,0.,-1.)) ;
#10297 = DIRECTION('',(1.,0.,0.)) ;
#10298 = DIRECTION('',(0.,0.,-1.)) ;
#10299 = DIRECTION('',(1.,0.,0.)) ;
#10300 = DIRECTION('',(0.,0.,-1.)) ;
#10301 = DIRECTION('center_axis',(-1.,0.,0.)) ;
#10302 = DIRECTION('ref_axis',(0.,0.,1.)) ;
#10303 = DIRECTION('',(0.,-1.,0.)) ;
#10304 = DIRECTION('',(0.,-1.,0.)) ;
#10305 = DIRECTION('',(0.,0.,-1.)) ;
#10306 = DIRECTION('center_axis',(0.,0.,1.)) ;
#10307 = DIRECTION('ref_axis',(1.,0.,0.)) ;
#10308 = DIRECTION('',(0.,1.,0.)) ;
#10309 = DIRECTION('',(-1.,0.,0.)) ;
#10310 = DIRECTION('center_axis',(0.,1.,0.)) ;
#10311 = DIRECTION('ref_axis',(0.,0.,1.)) ;
#10312 = DIRECTION('',(-1.,0.,0.)) ;
#10313 = DIRECTION('',(0.,0.,-1.)) ;
#10314 = DIRECTION('center_axis',(1.,0.,0.)) ;
#10315 = DIRECTION('ref_axis',(0.,0.,-1.)) ;
#10316 = DIRECTION('',(0.,1.,0.)) ;
#10317 = DIRECTION('center_axis',(0.,-1.,0.)) ;
#10318 = DIRECTION('ref_axis',(0.,0.,-1.)) ;
#10319 = DIRECTION('',(1.,0.,0.)) ;
#10320 = DIRECTION('',(0.,0.,-1.)) ;
#10321 = DIRECTION('',(1.,0.,0.)) ;
#10322 = DIRECTION('',(0.,0.,-1.)) ;
#10323 = DIRECTION('center_axis',(-1.,0.,0.)) ;
#10324 = DIRECTION('ref_axis',(0.,0.,1.)) ;
#10325 = DIRECTION('',(0.,-1.,0.)) ;
#10326 = DIRECTION('',(0.,-1.,0.)) ;
#10327 = DIRECTION('',(0.,0.,-1.)) ;
#10328 = DIRECTION('center_axis',(0.,0.,1.)) ;
#10329 = DIRECTION('ref_axis',(1.,0.,0.)) ;
#10330 = DIRECTION('',(0.,1.,0.)) ;
#10331 = DIRECTION('',(-1.,0.,0.)) ;
#10332 = DIRECTION('center_axis',(0.,1.,0.)) ;
#10333 = DIRECTION('ref_axis',(0.,0.,1.)) ;
#10334 = DIRECTION('',(-1.,0.,0.)) ;
#10335 = DIRECTION('',(0.,0.,-1.)) ;
#10336 = DIRECTION('center_axis',(1.,0.,0.)) ;
#10337 = DIRECTION('ref_axis',(0.,0.,-1.)) ;
#10338 = DIRECTION('',(0.,1.,0.)) ;
#10339 = DIRECTION('center_axis',(0.,-1.,0.)) ;
#10340 = DIRECTION('ref_axis',(0.,0.,-1.)) ;
#10341 = DIRECTION('',(1.,0.,0.)) ;
#10342 = DIRECTION('',(0.,0.,-1.)) ;
#10343 = DIRECTION('',(1.,0.,0.)) ;
#10344 = DIRECTION('',(0.,0.,-1.)) ;
#10345 = DIRECTION('center_axis',(-1.,0.,0.)) ;
#10346 = DIRECTION('ref_axis',(0.,0.,1.)) ;
#10347 = DIRECTION('',(0.,-1.,0.)) ;
#10348 = DIRECTION('',(0.,-1.,0.)) ;
#10349 = DIRECTION('',(0.,0.,-1.)) ;
#10350 = DIRECTION('center_axis',(0.,0.,1.)) ;
#10351 = DIRECTION('ref_axis',(1.,0.,0.)) ;
#10352 = DIRECTION('',(0.,1.,0.)) ;
#10353 = DIRECTION('',(-1.,0.,0.)) ;
#10354 = DIRECTION('center_axis',(0.,1.,0.)) ;
#10355 = DIRECTION('ref_axis',(0.,0.,1.)) ;
#10356 = DIRECTION('',(-1.,0.,0.)) ;
#10357 = DIRECTION('',(0.,0.,-1.)) ;
#10358 = DIRECTION('center_axis',(1.,0.,0.)) ;
#10359 = DIRECTION('ref_axis',(0.,0.,-1.)) ;
#10360 = DIRECTION('',(0.,1.,0.)) ;
#10361 = DIRECTION('center_axis',(0.,0.,1.)) ;
#10362 = DIRECTION('ref_axis',(1.,0.,0.)) ;
#10363 = DIRECTION('center_axis',(0.,0.,-1.)) ;
#10364 = DIRECTION('ref_axis',(1.,0.,0.)) ;
#10365 = DIRECTION('',(0.,0.,-1.)) ;
#10366 = DIRECTION('center_axis',(0.,0.,-1.)) ;
#10367 = DIRECTION('ref_axis',(1.,0.,0.)) ;
#10368 = DIRECTION('center_axis',(0.,0.,1.)) ;
#10369 = DIRECTION('ref_axis',(1.,0.,0.)) ;
#10370 = DIRECTION('center_axis',(0.,0.,1.)) ;
#10371 = DIRECTION('ref_axis',(1.,0.,0.)) ;
#10372 = DIRECTION('',(0.,0.,1.)) ;
#10373 = DIRECTION('center_axis',(0.,0.,1.)) ;
#10374 = DIRECTION('ref_axis',(1.,0.,0.)) ;
#10375 = DIRECTION('center_axis',(0.,0.,1.)) ;
#10376 = DIRECTION('ref_axis',(1.,0.,0.)) ;
#10377 = DIRECTION('center_axis',(0.,0.,-1.)) ;
#10378 = DIRECTION('ref_axis',(-1.,0.,0.)) ;
#10379 = DIRECTION('center_axis',(0.,0.,-1.)) ;
#10380 = DIRECTION('ref_axis',(1.,0.,0.)) ;
#10381 = DIRECTION('center_axis',(0.,0.,1.)) ;
#10382 = DIRECTION('ref_axis',(1.,0.,0.)) ;
#10383 = DIRECTION('center_axis',(0.,0.,-1.)) ;
#10384 = DIRECTION('ref_axis',(1.,0.,0.)) ;
#10385 = DIRECTION('',(0.,0.,-1.)) ;
#10386 = DIRECTION('center_axis',(0.,0.,1.)) ;
#10387 = DIRECTION('ref_axis',(1.,0.,0.)) ;
#10388 = DIRECTION('center_axis',(0.,0.,1.)) ;
#10389 = DIRECTION('ref_axis',(1.,0.,0.)) ;
#10390 = DIRECTION('',(0.,0.,1.)) ;
#10391 = DIRECTION('center_axis',(0.,0.,1.)) ;
#10392 = DIRECTION('ref_axis',(1.,0.,0.)) ;
#10393 = DIRECTION('center_axis',(0.,0.,1.)) ;
#10394 = DIRECTION('ref_axis',(1.,0.,0.)) ;
#10395 = DIRECTION('center_axis',(0.,0.,-1.)) ;
#10396 = DIRECTION('ref_axis',(-1.,0.,0.)) ;
#10397 = DIRECTION('center_axis',(0.,0.,-1.)) ;
#10398 = DIRECTION('ref_axis',(1.,0.,0.)) ;
#10399 = DIRECTION('center_axis',(0.,0.,1.)) ;
#10400 = DIRECTION('ref_axis',(1.,0.,0.)) ;
#10401 = DIRECTION('center_axis',(0.,0.,1.)) ;
#10402 = DIRECTION('ref_axis',(1.,0.,0.)) ;
#10403 = DIRECTION('',(0.,0.,-1.)) ;
#10404 = DIRECTION('center_axis',(0.,0.,-1.)) ;
#10405 = DIRECTION('ref_axis',(-1.,0.,0.)) ;
#10406 = DIRECTION('center_axis',(0.,0.,1.)) ;
#10407 = DIRECTION('ref_axis',(1.,0.,0.)) ;
#10408 = DIRECTION('axis',(0.,0.,1.)) ;
#10409 = DIRECTION('refdir',(1.,0.,0.)) ;
#10410 = DIRECTION('center_axis',(0.,0.,1.)) ;
#10411 = DIRECTION('ref_axis',(1.,0.,0.)) ;
#10412 = DIRECTION('center_axis',(0.,0.,1.)) ;
#10413 = DIRECTION('ref_axis',(1.,0.,0.)) ;
#10414 = DIRECTION('',(0.,0.,1.)) ;
#10415 = DIRECTION('center_axis',(0.,0.,-1.)) ;
#10416 = DIRECTION('ref_axis',(1.,0.,0.)) ;
#10417 = DIRECTION('center_axis',(0.,0.,1.)) ;
#10418 = DIRECTION('ref_axis',(1.,0.,0.)) ;
#10419 = DIRECTION('center_axis',(0.,0.,1.)) ;
#10420 = DIRECTION('ref_axis',(1.,0.,0.)) ;
#10421 = DIRECTION('',(0.,0.,-1.)) ;
#10422 = DIRECTION('center_axis',(0.,0.,-1.)) ;
#10423 = DIRECTION('ref_axis',(1.,0.,0.)) ;
#10424 = DIRECTION('center_axis',(0.,0.,-1.)) ;
#10425 = DIRECTION('ref_axis',(-1.,0.,0.)) ;
#10426 = DIRECTION('center_axis',(0.,0.,1.)) ;
#10427 = DIRECTION('ref_axis',(1.,0.,0.)) ;
#10428 = DIRECTION('axis',(0.,0.,1.)) ;
#10429 = DIRECTION('refdir',(1.,0.,0.)) ;
#10430 = DIRECTION('center_axis',(0.,0.,1.)) ;
#10431 = DIRECTION('ref_axis',(1.,0.,0.)) ;
#10432 = DIRECTION('center_axis',(0.,0.,1.)) ;
#10433 = DIRECTION('ref_axis',(1.,0.,0.)) ;
#10434 = DIRECTION('',(0.,0.,1.)) ;
#10435 = DIRECTION('center_axis',(0.,0.,-1.)) ;
#10436 = DIRECTION('ref_axis',(1.,0.,0.)) ;
#10437 = DIRECTION('center_axis',(0.,0.,1.)) ;
#10438 = DIRECTION('ref_axis',(1.,0.,0.)) ;
#10439 = DIRECTION('center_axis',(0.,0.,1.)) ;
#10440 = DIRECTION('ref_axis',(1.,0.,0.)) ;
#10441 = DIRECTION('',(0.,0.,-1.)) ;
#10442 = DIRECTION('center_axis',(0.,0.,-1.)) ;
#10443 = DIRECTION('ref_axis',(1.,0.,0.)) ;
#10444 = DIRECTION('center_axis',(0.,0.,-1.)) ;
#10445 = DIRECTION('ref_axis',(-1.,0.,0.)) ;
#10446 = DIRECTION('center_axis',(0.,0.,1.)) ;
#10447 = DIRECTION('ref_axis',(1.,0.,0.)) ;
#10448 = DIRECTION('axis',(0.,0.,1.)) ;
#10449 = DIRECTION('refdir',(1.,0.,0.)) ;
#10450 = DIRECTION('center_axis',(0.,0.,1.)) ;
#10451 = DIRECTION('ref_axis',(1.,0.,0.)) ;
#10452 = DIRECTION('center_axis',(0.,0.,-1.)) ;
#10453 = DIRECTION('ref_axis',(1.,0.,0.)) ;
#10454 = DIRECTION('center_axis',(1.22464679914735E-16,-1.,0.)) ;
#10455 = DIRECTION('ref_axis',(-1.,-1.22464679914735E-16,0.)) ;
#10456 = DIRECTION('center_axis',(0.,0.,1.)) ;
#10457 = DIRECTION('ref_axis',(1.,0.,0.)) ;
#10458 = DIRECTION('center_axis',(0.,0.,1.)) ;
#10459 = DIRECTION('ref_axis',(1.,0.,0.)) ;
#10460 = DIRECTION('',(0.,0.,-1.)) ;
#10461 = DIRECTION('center_axis',(0.,0.,1.)) ;
#10462 = DIRECTION('ref_axis',(1.,0.,0.)) ;
#10463 = DIRECTION('',(0.,0.,1.)) ;
#10464 = DIRECTION('',(1.,0.,0.)) ;
#10465 = DIRECTION('',(0.,0.,1.)) ;
#10466 = DIRECTION('',(1.,0.,0.)) ;
#10467 = DIRECTION('',(0.,0.,1.)) ;
#10468 = DIRECTION('',(1.,0.,0.)) ;
#10469 = DIRECTION('',(0.,0.,1.)) ;
#10470 = DIRECTION('',(1.,0.,0.)) ;
#10471 = DIRECTION('axis',(0.,0.,1.)) ;
#10472 = DIRECTION('refdir',(1.,0.,0.)) ;
#10473 = DIRECTION('axis',(0.,0.,1.)) ;
#10474 = DIRECTION('refdir',(1.,0.,0.)) ;
#10475 = DIRECTION('center_axis',(0.,0.,1.)) ;
#10476 = DIRECTION('ref_axis',(1.,0.,0.)) ;
#10477 = DIRECTION('center_axis',(0.,0.,1.)) ;
#10478 = DIRECTION('ref_axis',(1.,0.,0.)) ;
#10479 = DIRECTION('',(0.,0.,1.)) ;
#10480 = DIRECTION('center_axis',(0.,0.,-1.)) ;
#10481 = DIRECTION('ref_axis',(1.,0.,0.)) ;
#10482 = DIRECTION('center_axis',(0.,0.,1.)) ;
#10483 = DIRECTION('ref_axis',(1.,0.,0.)) ;
#10484 = DIRECTION('center_axis',(0.,0.,1.)) ;
#10485 = DIRECTION('ref_axis',(1.,0.,0.)) ;
#10486 = DIRECTION('',(0.,0.,1.)) ;
#10487 = DIRECTION('center_axis',(0.,0.,-1.)) ;
#10488 = DIRECTION('ref_axis',(1.,0.,0.)) ;
#10489 = DIRECTION('center_axis',(0.,0.,1.)) ;
#10490 = DIRECTION('ref_axis',(1.,0.,0.)) ;
#10491 = DIRECTION('center_axis',(0.,0.,1.)) ;
#10492 = DIRECTION('ref_axis',(1.,0.,0.)) ;
#10493 = DIRECTION('center_axis',(0.,0.,1.)) ;
#10494 = DIRECTION('ref_axis',(1.,0.,0.)) ;
#10495 = DIRECTION('',(0.,0.,-1.)) ;
#10496 = DIRECTION('center_axis',(0.,0.,-1.)) ;
#10497 = DIRECTION('ref_axis',(1.,0.,0.)) ;
#10498 = DIRECTION('center_axis',(0.,0.,-1.)) ;
#10499 = DIRECTION('ref_axis',(-1.,0.,0.)) ;
#10500 = DIRECTION('center_axis',(0.,0.,1.)) ;
#10501 = DIRECTION('ref_axis',(1.,0.,0.)) ;
#10502 = DIRECTION('axis',(0.,0.,1.)) ;
#10503 = DIRECTION('refdir',(1.,0.,0.)) ;
#10504 = DIRECTION('center_axis',(0.,0.,1.)) ;
#10505 = DIRECTION('ref_axis',(1.,0.,0.)) ;
#10506 = DIRECTION('center_axis',(0.,0.,1.)) ;
#10507 = DIRECTION('ref_axis',(1.,0.,0.)) ;
#10508 = DIRECTION('',(0.,0.,-1.)) ;
#10509 = DIRECTION('center_axis',(0.,0.,-1.)) ;
#10510 = DIRECTION('ref_axis',(1.,0.,0.)) ;
#10511 = DIRECTION('center_axis',(0.,0.,1.)) ;
#10512 = DIRECTION('ref_axis',(1.,0.,0.)) ;
#10513 = DIRECTION('center_axis',(0.,0.,1.)) ;
#10514 = DIRECTION('ref_axis',(1.,0.,0.)) ;
#10515 = DIRECTION('center_axis',(0.,0.,1.)) ;
#10516 = DIRECTION('ref_axis',(1.,0.,0.)) ;
#10517 = DIRECTION('',(0.,0.,-1.)) ;
#10518 = DIRECTION('center_axis',(0.,0.,-1.)) ;
#10519 = DIRECTION('ref_axis',(1.,0.,0.)) ;
#10520 = DIRECTION('center_axis',(0.,0.,-1.)) ;
#10521 = DIRECTION('ref_axis',(-1.,0.,0.)) ;
#10522 = DIRECTION('center_axis',(0.,0.,1.)) ;
#10523 = DIRECTION('ref_axis',(1.,0.,0.)) ;
#10524 = DIRECTION('axis',(0.,0.,1.)) ;
#10525 = DIRECTION('refdir',(1.,0.,0.)) ;
#10526 = DIRECTION('center_axis',(0.,0.,1.)) ;
#10527 = DIRECTION('ref_axis',(1.,0.,0.)) ;
#10528 = DIRECTION('center_axis',(0.,0.,1.)) ;
#10529 = DIRECTION('ref_axis',(1.,0.,0.)) ;
#10530 = DIRECTION('',(0.,0.,-1.)) ;
#10531 = DIRECTION('center_axis',(0.,0.,-1.)) ;
#10532 = DIRECTION('ref_axis',(1.,0.,0.)) ;
#10533 = DIRECTION('center_axis',(0.,0.,-1.)) ;
#10534 = DIRECTION('ref_axis',(-1.,0.,0.)) ;
#10535 = DIRECTION('center_axis',(0.,0.,1.)) ;
#10536 = DIRECTION('ref_axis',(1.,0.,0.)) ;
#10537 = DIRECTION('axis',(0.,0.,1.)) ;
#10538 = DIRECTION('refdir',(1.,0.,0.)) ;
#10539 = DIRECTION('center_axis',(1.,0.,0.)) ;
#10540 = DIRECTION('ref_axis',(0.,0.,-1.)) ;
#10541 = DIRECTION('',(0.,0.,1.)) ;
#10542 = DIRECTION('',(0.,1.,0.)) ;
#10543 = DIRECTION('',(0.,0.,-1.)) ;
#10544 = DIRECTION('',(0.,-1.,0.)) ;
#10545 = DIRECTION('center_axis',(0.,0.,1.)) ;
#10546 = DIRECTION('ref_axis',(1.,0.,0.)) ;
#10547 = DIRECTION('center_axis',(0.,0.,1.)) ;
#10548 = DIRECTION('ref_axis',(1.,0.,0.)) ;
#10549 = DIRECTION('',(0.,1.,0.)) ;
#10550 = DIRECTION('',(-1.,0.,0.)) ;
#10551 = DIRECTION('center_axis',(-1.,0.,0.)) ;
#10552 = DIRECTION('ref_axis',(0.,0.,1.)) ;
#10553 = DIRECTION('',(0.,0.,1.)) ;
#10554 = DIRECTION('',(0.,-1.,0.)) ;
#10555 = DIRECTION('',(0.,0.,-1.)) ;
#10556 = DIRECTION('center_axis',(0.,0.,1.)) ;
#10557 = DIRECTION('ref_axis',(1.,0.,0.)) ;
#10558 = DIRECTION('center_axis',(0.,0.,-1.)) ;
#10559 = DIRECTION('ref_axis',(1.,0.,0.)) ;
#10560 = DIRECTION('',(1.,0.,0.)) ;
#10561 = DIRECTION('center_axis',(0.,0.,1.)) ;
#10562 = DIRECTION('ref_axis',(1.,0.,0.)) ;
#10563 = DIRECTION('center_axis',(0.,0.,1.)) ;
#10564 = DIRECTION('ref_axis',(1.,0.,0.)) ;
#10565 = DIRECTION('',(-1.,0.,0.)) ;
#10566 = DIRECTION('center_axis',(0.,0.,1.)) ;
#10567 = DIRECTION('ref_axis',(1.,0.,0.)) ;
#10568 = DIRECTION('center_axis',(0.,0.,-1.)) ;
#10569 = DIRECTION('ref_axis',(1.,0.,0.)) ;
#10570 = DIRECTION('',(1.,0.,0.)) ;
#10571 = DIRECTION('center_axis',(0.,1.,0.)) ;
#10572 = DIRECTION('ref_axis',(0.,0.,1.)) ;
#10573 = DIRECTION('',(0.,0.,-1.)) ;
#10574 = DIRECTION('center_axis',(0.,-1.,0.)) ;
#10575 = DIRECTION('ref_axis',(0.,0.,-1.)) ;
#10576 = DIRECTION('',(0.,0.,-1.)) ;
#10577 = DIRECTION('center_axis',(0.,0.,1.)) ;
#10578 = DIRECTION('ref_axis',(1.,0.,0.)) ;
#10579 = DIRECTION('center_axis',(0.,0.,1.)) ;
#10580 = DIRECTION('ref_axis',(1.,0.,0.)) ;
#10581 = DIRECTION('',(0.,0.,1.)) ;
#10582 = DIRECTION('center_axis',(0.,0.,-1.)) ;
#10583 = DIRECTION('ref_axis',(1.,0.,0.)) ;
#10584 = DIRECTION('center_axis',(0.,0.,-1.)) ;
#10585 = DIRECTION('ref_axis',(-1.,0.,0.)) ;
#10586 = DIRECTION('center_axis',(0.,0.,1.)) ;
#10587 = DIRECTION('ref_axis',(1.,0.,0.)) ;
#10588 = DIRECTION('center_axis',(0.,0.,-1.)) ;
#10589 = DIRECTION('ref_axis',(1.,0.,0.)) ;
#10590 = DIRECTION('center_axis',(0.,0.,1.)) ;
#10591 = DIRECTION('ref_axis',(1.,0.,0.)) ;
#10592 = DIRECTION('',(0.,0.,-1.)) ;
#10593 = DIRECTION('center_axis',(0.,0.,1.)) ;
#10594 = DIRECTION('ref_axis',(1.,0.,0.)) ;
#10595 = DIRECTION('',(0.,0.,1.)) ;
#10596 = DIRECTION('center_axis',(0.,0.,-1.)) ;
#10597 = DIRECTION('ref_axis',(1.,0.,0.)) ;
#10598 = DIRECTION('center_axis',(0.,0.,1.)) ;
#10599 = DIRECTION('ref_axis',(1.,0.,0.)) ;
#10600 = DIRECTION('',(0.,0.,1.)) ;
#10601 = DIRECTION('center_axis',(0.,0.,1.)) ;
#10602 = DIRECTION('ref_axis',(1.,0.,0.)) ;
#10603 = DIRECTION('center_axis',(0.,0.,1.)) ;
#10604 = DIRECTION('ref_axis',(1.,0.,0.)) ;
#10605 = DIRECTION('',(0.,0.,1.)) ;
#10606 = DIRECTION('center_axis',(0.,0.,-1.)) ;
#10607 = DIRECTION('ref_axis',(1.,0.,0.)) ;
#10608 = DIRECTION('center_axis',(0.,0.,-1.)) ;
#10609 = DIRECTION('ref_axis',(1.,0.,0.)) ;
#10610 = DIRECTION('center_axis',(0.,0.,-1.)) ;
#10611 = DIRECTION('ref_axis',(-1.,0.,0.)) ;
#10612 = DIRECTION('center_axis',(0.,0.,1.)) ;
#10613 = DIRECTION('ref_axis',(1.,0.,0.)) ;
#10614 = DIRECTION('center_axis',(0.,0.,1.)) ;
#10615 = DIRECTION('ref_axis',(1.,0.,0.)) ;
#10616 = DIRECTION('center_axis',(0.,0.,1.)) ;
#10617 = DIRECTION('ref_axis',(1.,0.,0.)) ;
#10618 = DIRECTION('',(0.,0.,-1.)) ;
#10619 = DIRECTION('center_axis',(0.,0.,-1.)) ;
#10620 = DIRECTION('ref_axis',(1.,0.,0.)) ;
#10621 = DIRECTION('center_axis',(0.,0.,-1.)) ;
#10622 = DIRECTION('ref_axis',(-1.,0.,0.)) ;
#10623 = DIRECTION('axis',(0.,0.,1.)) ;
#10624 = DIRECTION('refdir',(1.,0.,0.)) ;
#10625 = DIRECTION('center_axis',(0.,0.,1.)) ;
#10626 = DIRECTION('ref_axis',(1.,0.,0.)) ;
#10627 = DIRECTION('center_axis',(0.,1.,0.)) ;
#10628 = DIRECTION('ref_axis',(-1.,0.,0.)) ;
#10629 = DIRECTION('center_axis',(0.,0.,1.)) ;
#10630 = DIRECTION('ref_axis',(1.,0.,0.)) ;
#10631 = DIRECTION('center_axis',(-1.,0.,0.)) ;
#10632 = DIRECTION('ref_axis',(0.,0.,-1.)) ;
#10633 = DIRECTION('center_axis',(0.,0.,1.)) ;
#10634 = DIRECTION('ref_axis',(1.,0.,0.)) ;
#10635 = DIRECTION('center_axis',(0.,0.,1.)) ;
#10636 = DIRECTION('ref_axis',(1.,0.,0.)) ;
#10637 = DIRECTION('center_axis',(-0.707106781186548,0.,-0.707106781186548)) ;
#10638 = DIRECTION('ref_axis',(0.707106781186548,0.,-0.707106781186548)) ;
#10639 = DIRECTION('center_axis',(1.,0.,0.)) ;
#10640 = DIRECTION('ref_axis',(0.,0.,-1.)) ;
#10641 = DIRECTION('center_axis',(0.,0.,-1.)) ;
#10642 = DIRECTION('ref_axis',(-1.,0.,0.)) ;
#10643 = DIRECTION('center_axis',(0.,0.,-1.)) ;
#10644 = DIRECTION('ref_axis',(1.,0.,0.)) ;
#10645 = DIRECTION('center_axis',(0.,0.,1.)) ;
#10646 = DIRECTION('ref_axis',(1.,0.,0.)) ;
#10647 = DIRECTION('center_axis',(0.,0.,1.)) ;
#10648 = DIRECTION('ref_axis',(1.,0.,0.)) ;
#10649 = DIRECTION('center_axis',(0.,0.,1.)) ;
#10650 = DIRECTION('ref_axis',(1.,0.,0.)) ;
#10651 = DIRECTION('center_axis',(0.,0.,1.)) ;
#10652 = DIRECTION('ref_axis',(1.,0.,0.)) ;
#10653 = DIRECTION('center_axis',(-0.707106781186548,0.,-0.707106781186548)) ;
#10654 = DIRECTION('ref_axis',(0.707106781186547,0.,-0.707106781186547)) ;
#10655 = DIRECTION('center_axis',(0.,0.,1.)) ;
#10656 = DIRECTION('ref_axis',(1.,0.,0.)) ;
#10657 = DIRECTION('',(0.,0.,-1.)) ;
#10658 = DIRECTION('center_axis',(0.,0.,1.)) ;
#10659 = DIRECTION('ref_axis',(1.,0.,0.)) ;
#10660 = DIRECTION('center_axis',(1.,0.,0.)) ;
#10661 = DIRECTION('ref_axis',(0.,0.,-1.)) ;
#10662 = DIRECTION('center_axis',(1.,0.,0.)) ;
#10663 = DIRECTION('ref_axis',(0.,0.,-1.)) ;
#10664 = DIRECTION('center_axis',(-1.,0.,0.)) ;
#10665 = DIRECTION('ref_axis',(0.,0.,-1.)) ;
#10666 = DIRECTION('center_axis',(1.,0.,0.)) ;
#10667 = DIRECTION('ref_axis',(0.,0.,-1.)) ;
#10668 = DIRECTION('center_axis',(-1.,0.,0.)) ;
#10669 = DIRECTION('ref_axis',(0.,0.,-1.)) ;
#10670 = DIRECTION('center_axis',(1.,0.,0.)) ;
#10671 = DIRECTION('ref_axis',(0.,0.,-1.)) ;
#10672 = DIRECTION('',(-1.,0.,0.)) ;
#10673 = DIRECTION('center_axis',(-1.,0.,0.)) ;
#10674 = DIRECTION('ref_axis',(0.,0.,-1.)) ;
#10675 = DIRECTION('center_axis',(-1.,0.,0.)) ;
#10676 = DIRECTION('ref_axis',(0.,0.,-1.)) ;
#10677 = DIRECTION('center_axis',(1.,0.,0.)) ;
#10678 = DIRECTION('ref_axis',(0.,0.,-1.)) ;
#10679 = DIRECTION('center_axis',(-1.,0.,0.)) ;
#10680 = DIRECTION('ref_axis',(0.,0.,-1.)) ;
#10681 = DIRECTION('',(1.,0.,0.)) ;
#10682 = DIRECTION('center_axis',(-1.,0.,0.)) ;
#10683 = DIRECTION('ref_axis',(0.,0.,-1.)) ;
#10684 = DIRECTION('center_axis',(0.,0.,1.)) ;
#10685 = DIRECTION('ref_axis',(1.,0.,0.)) ;
#10686 = DIRECTION('',(0.,0.,1.)) ;
#10687 = DIRECTION('center_axis',(0.,0.,1.)) ;
#10688 = DIRECTION('ref_axis',(1.,0.,0.)) ;
#10689 = DIRECTION('center_axis',(0.,0.,1.)) ;
#10690 = DIRECTION('ref_axis',(1.,0.,0.)) ;
#10691 = DIRECTION('center_axis',(0.577350269189626,0.577350269189626,0.577350269189626)) ;
#10692 = DIRECTION('ref_axis',(-0.707106781186548,0.,0.707106781186548)) ;
#10693 = DIRECTION('center_axis',(0.,0.,1.)) ;
#10694 = DIRECTION('ref_axis',(1.,0.,0.)) ;
#10695 = DIRECTION('center_axis',(1.,0.,0.)) ;
#10696 = DIRECTION('ref_axis',(0.,-1.,0.)) ;
#10697 = DIRECTION('axis',(0.,0.,1.)) ;
#10698 = DIRECTION('refdir',(1.,0.,0.)) ;
#10699 = DIRECTION('center_axis',(0.,0.,1.)) ;
#10700 = DIRECTION('ref_axis',(1.,0.,0.)) ;
#10701 = DIRECTION('center_axis',(0.,0.,1.)) ;
#10702 = DIRECTION('ref_axis',(1.,0.,0.)) ;
#10703 = DIRECTION('',(0.,0.,1.)) ;
#10704 = DIRECTION('center_axis',(0.,0.,-1.)) ;
#10705 = DIRECTION('ref_axis',(1.,0.,0.)) ;
#10706 = DIRECTION('center_axis',(0.,0.,1.)) ;
#10707 = DIRECTION('ref_axis',(1.,0.,0.)) ;
#10708 = DIRECTION('center_axis',(0.,0.,1.)) ;
#10709 = DIRECTION('ref_axis',(1.,0.,0.)) ;
#10710 = DIRECTION('',(0.,0.,-1.)) ;
#10711 = DIRECTION('center_axis',(0.,0.,-1.)) ;
#10712 = DIRECTION('ref_axis',(1.,0.,0.)) ;
#10713 = DIRECTION('center_axis',(0.,0.,-1.)) ;
#10714 = DIRECTION('ref_axis',(-1.,0.,0.)) ;
#10715 = DIRECTION('center_axis',(0.,0.,1.)) ;
#10716 = DIRECTION('ref_axis',(1.,0.,0.)) ;
#10717 = DIRECTION('axis',(0.,0.,1.)) ;
#10718 = DIRECTION('refdir',(1.,0.,0.)) ;
#10719 = DIRECTION('center_axis',(0.,0.,1.)) ;
#10720 = DIRECTION('ref_axis',(1.,0.,0.)) ;
#10721 = DIRECTION('center_axis',(0.,0.,1.)) ;
#10722 = DIRECTION('ref_axis',(1.,0.,0.)) ;
#10723 = DIRECTION('',(0.,0.,1.)) ;
#10724 = DIRECTION('center_axis',(0.,0.,-1.)) ;
#10725 = DIRECTION('ref_axis',(1.,0.,0.)) ;
#10726 = DIRECTION('center_axis',(0.,0.,1.)) ;
#10727 = DIRECTION('ref_axis',(1.,0.,0.)) ;
#10728 = DIRECTION('center_axis',(0.,0.,1.)) ;
#10729 = DIRECTION('ref_axis',(1.,0.,0.)) ;
#10730 = DIRECTION('',(0.,0.,1.)) ;
#10731 = DIRECTION('center_axis',(0.,0.,-1.)) ;
#10732 = DIRECTION('ref_axis',(1.,0.,0.)) ;
#10733 = DIRECTION('center_axis',(0.,0.,1.)) ;
#10734 = DIRECTION('ref_axis',(1.,0.,0.)) ;
#10735 = DIRECTION('center_axis',(0.,0.,1.)) ;
#10736 = DIRECTION('ref_axis',(1.,0.,0.)) ;
#10737 = DIRECTION('center_axis',(0.,0.,1.)) ;
#10738 = DIRECTION('ref_axis',(1.,0.,0.)) ;
#10739 = DIRECTION('',(0.,0.,-1.)) ;
#10740 = DIRECTION('center_axis',(0.,0.,-1.)) ;
#10741 = DIRECTION('ref_axis',(1.,0.,0.)) ;
#10742 = DIRECTION('center_axis',(0.,0.,-1.)) ;
#10743 = DIRECTION('ref_axis',(-1.,0.,0.)) ;
#10744 = DIRECTION('center_axis',(0.,0.,1.)) ;
#10745 = DIRECTION('ref_axis',(1.,0.,0.)) ;
#10746 = DIRECTION('axis',(0.,0.,1.)) ;
#10747 = DIRECTION('refdir',(1.,0.,0.)) ;
#10748 = DIRECTION('center_axis',(0.,0.,1.)) ;
#10749 = DIRECTION('ref_axis',(1.,0.,0.)) ;
#10750 = DIRECTION('center_axis',(0.,0.,1.)) ;
#10751 = DIRECTION('ref_axis',(1.,0.,0.)) ;
#10752 = DIRECTION('',(0.,0.,-1.)) ;
#10753 = DIRECTION('center_axis',(0.,0.,-1.)) ;
#10754 = DIRECTION('ref_axis',(1.,0.,0.)) ;
#10755 = DIRECTION('center_axis',(0.,0.,-1.)) ;
#10756 = DIRECTION('ref_axis',(-1.,0.,0.)) ;
#10757 = DIRECTION('center_axis',(0.,0.,1.)) ;
#10758 = DIRECTION('ref_axis',(1.,0.,0.)) ;
#10759 = DIRECTION('axis',(0.,0.,1.)) ;
#10760 = DIRECTION('refdir',(1.,0.,0.)) ;
#10761 = DIRECTION('center_axis',(0.,0.,1.)) ;
#10762 = DIRECTION('ref_axis',(1.,0.,0.)) ;
#10763 = DIRECTION('center_axis',(0.,0.,1.)) ;
#10764 = DIRECTION('ref_axis',(1.,0.,0.)) ;
#10765 = DIRECTION('',(0.,0.,-1.)) ;
#10766 = DIRECTION('center_axis',(0.,0.,-1.)) ;
#10767 = DIRECTION('ref_axis',(1.,0.,0.)) ;
#10768 = DIRECTION('center_axis',(0.,0.,-1.)) ;
#10769 = DIRECTION('ref_axis',(-1.,0.,0.)) ;
#10770 = DIRECTION('center_axis',(0.,0.,1.)) ;
#10771 = DIRECTION('ref_axis',(1.,0.,0.)) ;
#10772 = DIRECTION('',(0.,0.,1.)) ;
#10773 = DIRECTION('',(1.,0.,0.)) ;
#10774 = DIRECTION('',(0.,0.,1.)) ;
#10775 = DIRECTION('',(1.,0.,0.)) ;
#10776 = DIRECTION('',(0.,0.,1.)) ;
#10777 = DIRECTION('',(1.,0.,0.)) ;
#10778 = DIRECTION('',(0.,0.,1.)) ;
#10779 = DIRECTION('',(1.,0.,0.)) ;
#10780 = DIRECTION('',(0.,0.,1.)) ;
#10781 = DIRECTION('',(1.,0.,0.)) ;
#10782 = DIRECTION('',(0.,0.,1.)) ;
#10783 = DIRECTION('',(1.,0.,0.)) ;
#10784 = DIRECTION('',(0.,0.,1.)) ;
#10785 = DIRECTION('',(1.,0.,0.)) ;
#10786 = DIRECTION('',(0.,0.,1.)) ;
#10787 = DIRECTION('',(1.,0.,0.)) ;
#10788 = DIRECTION('',(0.,0.,1.)) ;
#10789 = DIRECTION('',(1.,0.,0.)) ;
#10790 = DIRECTION('axis',(0.,0.,1.)) ;
#10791 = DIRECTION('refdir',(1.,0.,0.)) ;
#10792 = DIRECTION('axis',(0.,0.,1.)) ;
#10793 = DIRECTION('refdir',(1.,0.,0.)) ;
#10794 = DIRECTION('center_axis',(0.,0.,1.)) ;
#10795 = DIRECTION('ref_axis',(1.,0.,0.)) ;
#10796 = DIRECTION('center_axis',(0.,0.,1.)) ;
#10797 = DIRECTION('ref_axis',(1.,0.,0.)) ;
#10798 = DIRECTION('',(0.,0.,1.)) ;
#10799 = DIRECTION('center_axis',(0.,0.,-1.)) ;
#10800 = DIRECTION('ref_axis',(1.,0.,0.)) ;
#10801 = DIRECTION('center_axis',(0.,0.,1.)) ;
#10802 = DIRECTION('ref_axis',(1.,0.,0.)) ;
#10803 = DIRECTION('',(0.,-1.,0.)) ;
#10804 = DIRECTION('',(-1.,0.,0.)) ;
#10805 = DIRECTION('',(0.,1.,0.)) ;
#10806 = DIRECTION('',(1.,0.,0.)) ;
#10807 = DIRECTION('center_axis',(1.,0.,0.)) ;
#10808 = DIRECTION('ref_axis',(0.,0.,-1.)) ;
#10809 = DIRECTION('',(0.,0.,-1.)) ;
#10810 = DIRECTION('',(0.,0.,-1.)) ;
#10811 = DIRECTION('',(0.,-1.,0.)) ;
#10812 = DIRECTION('center_axis',(-1.,0.,0.)) ;
#10813 = DIRECTION('ref_axis',(0.,0.,1.)) ;
#10814 = DIRECTION('',(0.,1.,0.)) ;
#10815 = DIRECTION('',(0.,0.,-1.)) ;
#10816 = DIRECTION('',(0.,0.,-1.)) ;
#10817 = DIRECTION('center_axis',(0.,1.,0.)) ;
#10818 = DIRECTION('ref_axis',(0.,0.,1.)) ;
#10819 = DIRECTION('',(-1.,0.,0.)) ;
#10820 = DIRECTION('center_axis',(0.,-1.,0.)) ;
#10821 = DIRECTION('ref_axis',(1.,0.,0.)) ;
#10822 = DIRECTION('',(-1.,0.,0.)) ;
#10823 = DIRECTION('',(0.,0.,-1.)) ;
#10824 = DIRECTION('',(1.,0.,0.)) ;
#10825 = DIRECTION('center_axis',(0.,-1.,0.)) ;
#10826 = DIRECTION('ref_axis',(1.,0.,0.)) ;
#10827 = DIRECTION('',(1.,0.,0.)) ;
#10828 = DIRECTION('center_axis',(0.,1.,0.)) ;
#10829 = DIRECTION('ref_axis',(1.,0.,0.)) ;
#10830 = DIRECTION('center_axis',(0.,0.,1.)) ;
#10831 = DIRECTION('ref_axis',(1.,0.,0.)) ;
#10832 = DIRECTION('',(1.,0.,0.)) ;
#10833 = DIRECTION('',(0.,-1.,0.)) ;
#10834 = DIRECTION('center_axis',(0.,1.,0.)) ;
#10835 = DIRECTION('ref_axis',(1.,0.,0.)) ;
#10836 = DIRECTION('',(0.,1.,0.)) ;
#10837 = DIRECTION('center_axis',(0.,-1.,0.)) ;
#10838 = DIRECTION('ref_axis',(1.,0.,0.)) ;
#10839 = DIRECTION('center_axis',(0.,1.,0.)) ;
#10840 = DIRECTION('ref_axis',(1.,0.,0.)) ;
#10841 = DIRECTION('center_axis',(0.,1.,0.)) ;
#10842 = DIRECTION('ref_axis',(1.,0.,0.)) ;
#10843 = DIRECTION('',(0.,1.,0.)) ;
#10844 = DIRECTION('center_axis',(0.,1.,0.)) ;
#10845 = DIRECTION('ref_axis',(1.,0.,0.)) ;
#10846 = DIRECTION('',(0.,1.,0.)) ;
#10847 = DIRECTION('',(0.,-1.,0.)) ;
#10848 = DIRECTION('center_axis',(0.,1.,0.)) ;
#10849 = DIRECTION('ref_axis',(1.,0.,0.)) ;
#10850 = DIRECTION('center_axis',(0.,0.,1.)) ;
#10851 = DIRECTION('ref_axis',(1.,0.,0.)) ;
#10852 = DIRECTION('',(0.,1.,0.)) ;
#10853 = DIRECTION('',(-1.,0.,0.)) ;
#10854 = DIRECTION('center_axis',(0.,0.,1.)) ;
#10855 = DIRECTION('ref_axis',(1.,0.,0.)) ;
#10856 = DIRECTION('',(-1.,0.,0.)) ;
#10857 = DIRECTION('center_axis',(0.,-1.,0.)) ;
#10858 = DIRECTION('ref_axis',(0.,0.,-1.)) ;
#10859 = DIRECTION('',(0.,0.,-1.)) ;
#10860 = DIRECTION('',(1.,0.,0.)) ;
#10861 = DIRECTION('center_axis',(0.,0.,1.)) ;
#10862 = DIRECTION('ref_axis',(1.,0.,0.)) ;
#10863 = DIRECTION('',(0.,-1.,0.)) ;
#10864 = DIRECTION('center_axis',(-1.,0.,0.)) ;
#10865 = DIRECTION('ref_axis',(0.,0.,1.)) ;
#10866 = DIRECTION('axis',(0.,0.,1.)) ;
#10867 = DIRECTION('refdir',(1.,0.,0.)) ;
#10868 = DIRECTION('center_axis',(0.,1.,0.)) ;
#10869 = DIRECTION('ref_axis',(1.,0.,0.)) ;
#10870 = DIRECTION('center_axis',(0.,1.,0.)) ;
#10871 = DIRECTION('ref_axis',(1.,0.,0.)) ;
#10872 = DIRECTION('center_axis',(0.,-1.,0.)) ;
#10873 = DIRECTION('ref_axis',(1.,0.,0.)) ;
#10874 = DIRECTION('center_axis',(0.,1.,0.)) ;
#10875 = DIRECTION('ref_axis',(1.,0.,0.)) ;
#10876 = DIRECTION('',(0.,-1.,0.)) ;
#10877 = DIRECTION('center_axis',(0.,-1.,0.)) ;
#10878 = DIRECTION('ref_axis',(1.,0.,0.)) ;
#10879 = DIRECTION('center_axis',(0.,-1.,0.)) ;
#10880 = DIRECTION('ref_axis',(-1.,0.,0.)) ;
#10881 = DIRECTION('center_axis',(0.,1.,0.)) ;
#10882 = DIRECTION('ref_axis',(1.,0.,0.)) ;
#10883 = DIRECTION('center_axis',(0.,1.,0.)) ;
#10884 = DIRECTION('ref_axis',(1.,0.,0.)) ;
#10885 = DIRECTION('',(0.,-1.,0.)) ;
#10886 = DIRECTION('center_axis',(0.,1.,0.)) ;
#10887 = DIRECTION('ref_axis',(1.,0.,0.)) ;
#10888 = DIRECTION('axis',(0.,0.,1.)) ;
#10889 = DIRECTION('refdir',(1.,0.,0.)) ;
#10890 = DIRECTION('center_axis',(0.,0.,1.)) ;
#10891 = DIRECTION('ref_axis',(1.,0.,0.)) ;
#10892 = DIRECTION('center_axis',(-0.376865806842073,-0.909834542072809,-0.173704547103507)) ;
#10893 = DIRECTION('ref_axis',(0.926267868185695,-0.370179664617619,-0.0706742687992891)) ;
#10894 = DIRECTION('center_axis',(0.909834542072811,0.376865806842069,0.17370454710351)) ;
#10895 = DIRECTION('ref_axis',(0.414971211111276,-0.826287510096955,-0.380851473157994)) ;
#10896 = DIRECTION('center_axis',(0.,0.,1.)) ;
#10897 = DIRECTION('ref_axis',(1.,0.,0.)) ;
#10898 = DIRECTION('center_axis',(-0.909834542072811,-0.376865806842069,-0.17370454710351)) ;
#10899 = DIRECTION('ref_axis',(0.414971211111276,-0.826287510096955,-0.380851473157994)) ;
#10900 = DIRECTION('center_axis',(0.909834542072809,-0.376865806842073,0.173704547103512)) ;
#10901 = DIRECTION('ref_axis',(0.41497121111128,0.826287510096954,-0.380851473157994)) ;
#10902 = DIRECTION('center_axis',(0.909834542072809,-0.376865806842073,0.173704547103512)) ;
#10903 = DIRECTION('ref_axis',(0.41497121111128,0.826287510096954,-0.380851473157994)) ;
#10904 = DIRECTION('center_axis',(0.,0.,1.)) ;
#10905 = DIRECTION('ref_axis',(-0.707106781186536,-0.707106781186559,0.)) ;
#10906 = DIRECTION('center_axis',(-0.909834542072809,0.376865806842073,-0.173704547103512)) ;
#10907 = DIRECTION('ref_axis',(0.41497121111128,0.826287510096954,-0.380851473157994)) ;
#10908 = DIRECTION('center_axis',(-0.909834542072809,0.376865806842073,-0.173704547103512)) ;
#10909 = DIRECTION('ref_axis',(0.41497121111128,0.826287510096954,-0.380851473157994)) ;
#10910 = DIRECTION('center_axis',(0.376865806842071,-0.90983454207281,0.173704547103507)) ;
#10911 = DIRECTION('ref_axis',(0.926267868185696,0.370179664617617,-0.0706742687992885)) ;
#10912 = DIRECTION('center_axis',(0.376865806842071,-0.90983454207281,0.173704547103507)) ;
#10913 = DIRECTION('ref_axis',(0.926267868185696,0.370179664617617,-0.0706742687992885)) ;
#10914 = DIRECTION('center_axis',(0.,0.,1.)) ;
#10915 = DIRECTION('ref_axis',(-1.,0.,0.)) ;
#10916 = DIRECTION('center_axis',(-0.376865806842071,0.90983454207281,-0.173704547103507)) ;
#10917 = DIRECTION('ref_axis',(0.926267868185696,0.370179664617617,-0.0706742687992885)) ;
#10918 = DIRECTION('center_axis',(-0.376865806842071,0.90983454207281,-0.173704547103507)) ;
#10919 = DIRECTION('ref_axis',(0.926267868185696,0.370179664617617,-0.0706742687992885)) ;
#10920 = DIRECTION('center_axis',(-0.376865806842073,-0.909834542072809,0.173704547103509)) ;
#10921 = DIRECTION('ref_axis',(0.926267868185696,-0.370179664617619,0.0706742687992895)) ;
#10922 = DIRECTION('center_axis',(-0.376865806842073,-0.909834542072809,0.173704547103509)) ;
#10923 = DIRECTION('ref_axis',(0.926267868185696,-0.370179664617619,0.0706742687992895)) ;
#10924 = DIRECTION('center_axis',(0.,0.,1.)) ;
#10925 = DIRECTION('ref_axis',(-0.707106781186554,0.707106781186541,0.)) ;
#10926 = DIRECTION('center_axis',(0.376865806842073,0.909834542072809,-0.173704547103509)) ;
#10927 = DIRECTION('ref_axis',(0.926267868185696,-0.370179664617619,0.0706742687992895)) ;
#10928 = DIRECTION('center_axis',(0.376865806842073,0.909834542072809,-0.173704547103509)) ;
#10929 = DIRECTION('ref_axis',(0.926267868185696,-0.370179664617619,0.0706742687992895)) ;
#10930 = DIRECTION('center_axis',(-0.90983454207281,-0.376865806842072,0.173704547103508)) ;
#10931 = DIRECTION('ref_axis',(0.414971211111278,-0.826287510096957,0.38085147315799)) ;
#10932 = DIRECTION('center_axis',(-0.90983454207281,-0.376865806842072,0.173704547103508)) ;
#10933 = DIRECTION('ref_axis',(0.414971211111278,-0.826287510096957,0.38085147315799)) ;
#10934 = DIRECTION('center_axis',(0.,0.,1.)) ;
#10935 = DIRECTION('ref_axis',(1.,0.,0.)) ;
#10936 = DIRECTION('center_axis',(0.90983454207281,0.376865806842072,-0.173704547103508)) ;
#10937 = DIRECTION('ref_axis',(0.414971211111278,-0.826287510096957,0.38085147315799)) ;
#10938 = DIRECTION('center_axis',(0.90983454207281,0.376865806842072,-0.173704547103508)) ;
#10939 = DIRECTION('ref_axis',(0.414971211111278,-0.826287510096957,0.38085147315799)) ;
#10940 = DIRECTION('center_axis',(-0.909834542072809,0.376865806842072,0.173704547103511)) ;
#10941 = DIRECTION('ref_axis',(0.414971211111279,0.826287510096954,0.380851473157994)) ;
#10942 = DIRECTION('center_axis',(0.,0.,1.)) ;
#10943 = DIRECTION('ref_axis',(1.,0.,0.)) ;
#10944 = DIRECTION('center_axis',(0.909834542072809,-0.376865806842072,-0.173704547103511)) ;
#10945 = DIRECTION('ref_axis',(0.414971211111279,0.826287510096954,0.380851473157994)) ;
#10946 = DIRECTION('center_axis',(-0.376865806842072,0.909834542072809,0.17370454710351)) ;
#10947 = DIRECTION('ref_axis',(0.926267868185696,0.370179664617617,0.0706742687992896)) ;
#10948 = DIRECTION('center_axis',(0.,0.,1.)) ;
#10949 = DIRECTION('ref_axis',(1.,0.,0.)) ;
#10950 = DIRECTION('center_axis',(0.376865806842072,-0.909834542072809,-0.17370454710351)) ;
#10951 = DIRECTION('ref_axis',(0.926267868185696,0.370179664617617,0.0706742687992896)) ;
#10952 = DIRECTION('center_axis',(0.376865806842073,0.909834542072809,0.173704547103507)) ;
#10953 = DIRECTION('ref_axis',(0.926267868185695,-0.370179664617619,-0.0706742687992891)) ;
#10954 = DIRECTION('center_axis',(0.,0.,1.)) ;
#10955 = DIRECTION('ref_axis',(1.,0.,0.)) ;
#10956 = DIRECTION('center_axis',(-0.376865806842073,-0.909834542072809,-0.173704547103507)) ;
#10957 = DIRECTION('ref_axis',(0.926267868185695,-0.370179664617619,-0.0706742687992891)) ;
#10958 = DIRECTION('center_axis',(0.909834542072811,0.376865806842069,0.17370454710351)) ;
#10959 = DIRECTION('ref_axis',(0.414971211111276,-0.826287510096955,-0.380851473157994)) ;
#10960 = DIRECTION('center_axis',(0.,0.,1.)) ;
#10961 = DIRECTION('ref_axis',(1.,0.,0.)) ;
#10962 = DIRECTION('center_axis',(-0.909834542072811,-0.376865806842069,-0.17370454710351)) ;
#10963 = DIRECTION('ref_axis',(0.414971211111276,-0.826287510096955,-0.380851473157994)) ;
#10964 = DIRECTION('center_axis',(0.909834542072809,-0.376865806842073,0.173704547103508)) ;
#10965 = DIRECTION('ref_axis',(0.414971211111279,0.826287510096957,-0.380851473157988)) ;
#10966 = DIRECTION('center_axis',(0.909834542072809,-0.376865806842073,0.173704547103508)) ;
#10967 = DIRECTION('ref_axis',(0.414971211111279,0.826287510096957,-0.380851473157988)) ;
#10968 = DIRECTION('center_axis',(0.,0.,1.)) ;
#10969 = DIRECTION('ref_axis',(-0.707106781186543,-0.707106781186552,0.)) ;
#10970 = DIRECTION('center_axis',(-0.909834542072809,0.376865806842073,-0.173704547103508)) ;
#10971 = DIRECTION('ref_axis',(0.414971211111279,0.826287510096957,-0.380851473157988)) ;
#10972 = DIRECTION('center_axis',(-0.909834542072809,0.376865806842073,-0.173704547103508)) ;
#10973 = DIRECTION('ref_axis',(0.414971211111279,0.826287510096957,-0.380851473157988)) ;
#10974 = DIRECTION('center_axis',(0.376865806842071,-0.90983454207281,0.17370454710351)) ;
#10975 = DIRECTION('ref_axis',(0.926267868185696,0.370179664617617,-0.0706742687992895)) ;
#10976 = DIRECTION('center_axis',(0.376865806842071,-0.90983454207281,0.17370454710351)) ;
#10977 = DIRECTION('ref_axis',(0.926267868185696,0.370179664617617,-0.0706742687992895)) ;
#10978 = DIRECTION('center_axis',(0.,0.,1.)) ;
#10979 = DIRECTION('ref_axis',(-1.,0.,0.)) ;
#10980 = DIRECTION('center_axis',(-0.376865806842071,0.90983454207281,-0.17370454710351)) ;
#10981 = DIRECTION('ref_axis',(0.926267868185696,0.370179664617617,-0.0706742687992895)) ;
#10982 = DIRECTION('center_axis',(-0.376865806842071,0.90983454207281,-0.17370454710351)) ;
#10983 = DIRECTION('ref_axis',(0.926267868185696,0.370179664617617,-0.0706742687992895)) ;
#10984 = DIRECTION('center_axis',(-0.376865806842073,-0.909834542072809,0.173704547103508)) ;
#10985 = DIRECTION('ref_axis',(0.926267868185696,-0.370179664617619,0.0706742687992894)) ;
#10986 = DIRECTION('center_axis',(-0.376865806842073,-0.909834542072809,0.173704547103508)) ;
#10987 = DIRECTION('ref_axis',(0.926267868185696,-0.370179664617619,0.0706742687992894)) ;
#10988 = DIRECTION('center_axis',(0.,0.,1.)) ;
#10989 = DIRECTION('ref_axis',(-0.707106781186554,0.707106781186541,0.)) ;
#10990 = DIRECTION('center_axis',(0.376865806842073,0.909834542072809,-0.173704547103508)) ;
#10991 = DIRECTION('ref_axis',(0.926267868185696,-0.370179664617619,0.0706742687992894)) ;
#10992 = DIRECTION('center_axis',(0.376865806842073,0.909834542072809,-0.173704547103508)) ;
#10993 = DIRECTION('ref_axis',(0.926267868185696,-0.370179664617619,0.0706742687992894)) ;
#10994 = DIRECTION('center_axis',(-0.909834542072809,-0.376865806842072,0.17370454710351)) ;
#10995 = DIRECTION('ref_axis',(0.414971211111279,-0.826287510096955,0.380851473157994)) ;
#10996 = DIRECTION('center_axis',(-0.909834542072809,-0.376865806842072,0.17370454710351)) ;
#10997 = DIRECTION('ref_axis',(0.414971211111279,-0.826287510096955,0.380851473157994)) ;
#10998 = DIRECTION('center_axis',(0.,0.,1.)) ;
#10999 = DIRECTION('ref_axis',(1.,0.,0.)) ;
#11000 = DIRECTION('center_axis',(0.909834542072809,0.376865806842072,-0.17370454710351)) ;
#11001 = DIRECTION('ref_axis',(0.414971211111279,-0.826287510096955,0.380851473157994)) ;
#11002 = DIRECTION('center_axis',(0.909834542072809,0.376865806842072,-0.17370454710351)) ;
#11003 = DIRECTION('ref_axis',(0.414971211111279,-0.826287510096955,0.380851473157994)) ;
#11004 = DIRECTION('center_axis',(-0.90983454207281,0.376865806842072,0.173704547103509)) ;
#11005 = DIRECTION('ref_axis',(0.414971211111278,0.826287510096956,0.38085147315799)) ;
#11006 = DIRECTION('center_axis',(0.,0.,1.)) ;
#11007 = DIRECTION('ref_axis',(1.,0.,0.)) ;
#11008 = DIRECTION('center_axis',(0.90983454207281,-0.376865806842072,-0.173704547103509)) ;
#11009 = DIRECTION('ref_axis',(0.414971211111278,0.826287510096956,0.38085147315799)) ;
#11010 = DIRECTION('center_axis',(-0.376865806842072,0.909834542072809,0.173704547103509)) ;
#11011 = DIRECTION('ref_axis',(0.926267868185696,0.370179664617618,0.0706742687992892)) ;
#11012 = DIRECTION('center_axis',(0.,0.,1.)) ;
#11013 = DIRECTION('ref_axis',(1.,0.,0.)) ;
#11014 = DIRECTION('center_axis',(0.376865806842072,-0.909834542072809,-0.173704547103509)) ;
#11015 = DIRECTION('ref_axis',(0.926267868185696,0.370179664617618,0.0706742687992892)) ;
#11016 = DIRECTION('center_axis',(0.376865806842073,0.909834542072809,0.173704547103509)) ;
#11017 = DIRECTION('ref_axis',(0.926267868185696,-0.370179664617619,-0.0706742687992895)) ;
#11018 = DIRECTION('center_axis',(0.,0.,1.)) ;
#11019 = DIRECTION('ref_axis',(1.,0.,0.)) ;
#11020 = DIRECTION('center_axis',(-0.376865806842073,-0.909834542072809,-0.173704547103509)) ;
#11021 = DIRECTION('ref_axis',(0.926267868185696,-0.370179664617619,-0.0706742687992895)) ;
#11022 = DIRECTION('center_axis',(0.90983454207281,0.37686580684207,0.173704547103509)) ;
#11023 = DIRECTION('ref_axis',(0.414971211111277,-0.826287510096957,-0.380851473157992)) ;
#11024 = DIRECTION('center_axis',(0.,0.,1.)) ;
#11025 = DIRECTION('ref_axis',(1.,0.,0.)) ;
#11026 = DIRECTION('center_axis',(-0.90983454207281,-0.37686580684207,-0.173704547103509)) ;
#11027 = DIRECTION('ref_axis',(0.414971211111277,-0.826287510096957,-0.380851473157992)) ;
#11028 = DIRECTION('center_axis',(0.909834542072809,-0.376865806842073,0.17370454710351)) ;
#11029 = DIRECTION('ref_axis',(0.41497121111128,0.826287510096955,-0.380851473157992)) ;
#11030 = DIRECTION('center_axis',(0.909834542072809,-0.376865806842073,0.17370454710351)) ;
#11031 = DIRECTION('ref_axis',(0.41497121111128,0.826287510096955,-0.380851473157992)) ;
#11032 = DIRECTION('center_axis',(0.,0.,1.)) ;
#11033 = DIRECTION('ref_axis',(-0.707106781186556,-0.707106781186539,0.)) ;
#11034 = DIRECTION('center_axis',(-0.909834542072809,0.376865806842073,-0.17370454710351)) ;
#11035 = DIRECTION('ref_axis',(0.41497121111128,0.826287510096955,-0.380851473157992)) ;
#11036 = DIRECTION('center_axis',(-0.909834542072809,0.376865806842073,-0.17370454710351)) ;
#11037 = DIRECTION('ref_axis',(0.41497121111128,0.826287510096955,-0.380851473157992)) ;
#11038 = DIRECTION('center_axis',(0.376865806842071,-0.90983454207281,0.173704547103509)) ;
#11039 = DIRECTION('ref_axis',(0.926267868185696,0.370179664617617,-0.070674268799289)) ;
#11040 = DIRECTION('center_axis',(0.376865806842071,-0.90983454207281,0.173704547103509)) ;
#11041 = DIRECTION('ref_axis',(0.926267868185696,0.370179664617617,-0.070674268799289)) ;
#11042 = DIRECTION('center_axis',(0.,0.,1.)) ;
#11043 = DIRECTION('ref_axis',(-1.,2.22044604925032E-14,0.)) ;
#11044 = DIRECTION('center_axis',(-0.376865806842071,0.90983454207281,-0.173704547103509)) ;
#11045 = DIRECTION('ref_axis',(0.926267868185696,0.370179664617617,-0.070674268799289)) ;
#11046 = DIRECTION('center_axis',(-0.376865806842071,0.90983454207281,-0.173704547103509)) ;
#11047 = DIRECTION('ref_axis',(0.926267868185696,0.370179664617617,-0.070674268799289)) ;
#11048 = DIRECTION('center_axis',(-0.376865806842073,-0.909834542072809,0.17370454710351)) ;
#11049 = DIRECTION('ref_axis',(0.926267868185696,-0.370179664617618,0.0706742687992898)) ;
#11050 = DIRECTION('center_axis',(-0.376865806842073,-0.909834542072809,0.17370454710351)) ;
#11051 = DIRECTION('ref_axis',(0.926267868185696,-0.370179664617618,0.0706742687992898)) ;
#11052 = DIRECTION('center_axis',(0.,0.,1.)) ;
#11053 = DIRECTION('ref_axis',(-0.707106781186572,0.707106781186523,0.)) ;
#11054 = DIRECTION('center_axis',(0.376865806842073,0.909834542072809,-0.17370454710351)) ;
#11055 = DIRECTION('ref_axis',(0.926267868185696,-0.370179664617618,0.0706742687992898)) ;
#11056 = DIRECTION('center_axis',(0.376865806842073,0.909834542072809,-0.17370454710351)) ;
#11057 = DIRECTION('ref_axis',(0.926267868185696,-0.370179664617618,0.0706742687992898)) ;
#11058 = DIRECTION('center_axis',(-0.90983454207281,-0.376865806842071,0.173704547103508)) ;
#11059 = DIRECTION('ref_axis',(0.414971211111277,-0.826287510096957,0.38085147315799)) ;
#11060 = DIRECTION('center_axis',(-0.90983454207281,-0.376865806842071,0.173704547103508)) ;
#11061 = DIRECTION('ref_axis',(0.414971211111277,-0.826287510096957,0.38085147315799)) ;
#11062 = DIRECTION('center_axis',(0.,0.,1.)) ;
#11063 = DIRECTION('ref_axis',(1.,0.,0.)) ;
#11064 = DIRECTION('center_axis',(0.90983454207281,0.376865806842071,-0.173704547103508)) ;
#11065 = DIRECTION('ref_axis',(0.414971211111277,-0.826287510096957,0.38085147315799)) ;
#11066 = DIRECTION('center_axis',(0.90983454207281,0.376865806842071,-0.173704547103508)) ;
#11067 = DIRECTION('ref_axis',(0.414971211111277,-0.826287510096957,0.38085147315799)) ;
#11068 = DIRECTION('center_axis',(-0.909834542072809,0.376865806842072,0.17370454710351)) ;
#11069 = DIRECTION('ref_axis',(0.414971211111279,0.826287510096955,0.380851473157992)) ;
#11070 = DIRECTION('center_axis',(0.,0.,1.)) ;
#11071 = DIRECTION('ref_axis',(1.,0.,0.)) ;
#11072 = DIRECTION('center_axis',(0.909834542072809,-0.376865806842072,-0.17370454710351)) ;
#11073 = DIRECTION('ref_axis',(0.414971211111279,0.826287510096955,0.380851473157992)) ;
#11074 = DIRECTION('center_axis',(-0.376865806842072,0.909834542072809,0.173704547103509)) ;
#11075 = DIRECTION('ref_axis',(0.926267868185696,0.370179664617618,0.0706742687992893)) ;
#11076 = DIRECTION('center_axis',(0.,0.,1.)) ;
#11077 = DIRECTION('ref_axis',(1.,0.,0.)) ;
#11078 = DIRECTION('center_axis',(0.376865806842072,-0.909834542072809,-0.173704547103509)) ;
#11079 = DIRECTION('ref_axis',(0.926267868185696,0.370179664617618,0.0706742687992893)) ;
#11080 = DIRECTION('center_axis',(0.376865806842073,0.909834542072809,0.17370454710351)) ;
#11081 = DIRECTION('ref_axis',(0.926267868185696,-0.370179664617619,-0.0706742687992899)) ;
#11082 = DIRECTION('center_axis',(0.,0.,1.)) ;
#11083 = DIRECTION('ref_axis',(1.,0.,0.)) ;
#11084 = DIRECTION('center_axis',(-0.376865806842073,-0.909834542072809,-0.17370454710351)) ;
#11085 = DIRECTION('ref_axis',(0.926267868185696,-0.370179664617619,-0.0706742687992899)) ;
#11086 = DIRECTION('center_axis',(0.90983454207281,0.376865806842072,0.173704547103509)) ;
#11087 = DIRECTION('ref_axis',(0.414971211111278,-0.826287510096956,-0.380851473157991)) ;
#11088 = DIRECTION('center_axis',(0.,0.,1.)) ;
#11089 = DIRECTION('ref_axis',(1.,0.,0.)) ;
#11090 = DIRECTION('center_axis',(-0.90983454207281,-0.376865806842072,-0.173704547103509)) ;
#11091 = DIRECTION('ref_axis',(0.414971211111278,-0.826287510096956,-0.380851473157991)) ;
#11092 = DIRECTION('center_axis',(0.90983454207281,-0.376865806842072,0.173704547103508)) ;
#11093 = DIRECTION('ref_axis',(0.414971211111278,0.826287510096957,-0.380851473157989)) ;
#11094 = DIRECTION('center_axis',(0.90983454207281,-0.376865806842072,0.173704547103508)) ;
#11095 = DIRECTION('ref_axis',(0.414971211111278,0.826287510096957,-0.380851473157989)) ;
#11096 = DIRECTION('center_axis',(0.,0.,1.)) ;
#11097 = DIRECTION('ref_axis',(-0.707106781186543,-0.707106781186552,0.)) ;
#11098 = DIRECTION('center_axis',(-0.90983454207281,0.376865806842072,-0.173704547103508)) ;
#11099 = DIRECTION('ref_axis',(0.414971211111278,0.826287510096957,-0.380851473157989)) ;
#11100 = DIRECTION('center_axis',(-0.90983454207281,0.376865806842072,-0.173704547103508)) ;
#11101 = DIRECTION('ref_axis',(0.414971211111278,0.826287510096957,-0.380851473157989)) ;
#11102 = DIRECTION('center_axis',(0.376865806842071,-0.90983454207281,0.173704547103509)) ;
#11103 = DIRECTION('ref_axis',(0.926267868185696,0.370179664617617,-0.0706742687992893)) ;
#11104 = DIRECTION('center_axis',(0.376865806842071,-0.90983454207281,0.173704547103509)) ;
#11105 = DIRECTION('ref_axis',(0.926267868185696,0.370179664617617,-0.0706742687992893)) ;
#11106 = DIRECTION('center_axis',(0.,0.,1.)) ;
#11107 = DIRECTION('ref_axis',(-1.,0.,0.)) ;
#11108 = DIRECTION('center_axis',(-0.376865806842071,0.90983454207281,-0.173704547103509)) ;
#11109 = DIRECTION('ref_axis',(0.926267868185696,0.370179664617617,-0.0706742687992893)) ;
#11110 = DIRECTION('center_axis',(-0.376865806842071,0.90983454207281,-0.173704547103509)) ;
#11111 = DIRECTION('ref_axis',(0.926267868185696,0.370179664617617,-0.0706742687992893)) ;
#11112 = DIRECTION('center_axis',(-0.376865806842073,-0.909834542072809,0.173704547103509)) ;
#11113 = DIRECTION('ref_axis',(0.926267868185696,-0.370179664617619,0.0706742687992897)) ;
#11114 = DIRECTION('center_axis',(-0.376865806842073,-0.909834542072809,0.173704547103509)) ;
#11115 = DIRECTION('ref_axis',(0.926267868185696,-0.370179664617619,0.0706742687992897)) ;
#11116 = DIRECTION('center_axis',(0.,0.,1.)) ;
#11117 = DIRECTION('ref_axis',(-0.707106781186574,0.707106781186521,0.)) ;
#11118 = DIRECTION('center_axis',(0.376865806842073,0.909834542072809,-0.173704547103509)) ;
#11119 = DIRECTION('ref_axis',(0.926267868185696,-0.370179664617619,0.0706742687992897)) ;
#11120 = DIRECTION('center_axis',(0.376865806842073,0.909834542072809,-0.173704547103509)) ;
#11121 = DIRECTION('ref_axis',(0.926267868185696,-0.370179664617619,0.0706742687992897)) ;
#11122 = DIRECTION('center_axis',(-0.90983454207281,-0.376865806842072,0.17370454710351)) ;
#11123 = DIRECTION('ref_axis',(0.414971211111278,-0.826287510096955,0.380851473157992)) ;
#11124 = DIRECTION('center_axis',(-0.90983454207281,-0.376865806842072,0.17370454710351)) ;
#11125 = DIRECTION('ref_axis',(0.414971211111278,-0.826287510096955,0.380851473157992)) ;
#11126 = DIRECTION('center_axis',(0.,0.,1.)) ;
#11127 = DIRECTION('ref_axis',(1.,0.,0.)) ;
#11128 = DIRECTION('center_axis',(0.90983454207281,0.376865806842072,-0.17370454710351)) ;
#11129 = DIRECTION('ref_axis',(0.414971211111278,-0.826287510096955,0.380851473157992)) ;
#11130 = DIRECTION('center_axis',(0.90983454207281,0.376865806842072,-0.17370454710351)) ;
#11131 = DIRECTION('ref_axis',(0.414971211111278,-0.826287510096955,0.380851473157992)) ;
#11132 = DIRECTION('center_axis',(-0.909834542072809,0.376865806842072,0.173704547103509)) ;
#11133 = DIRECTION('ref_axis',(0.414971211111278,0.826287510096956,0.38085147315799)) ;
#11134 = DIRECTION('center_axis',(0.,0.,1.)) ;
#11135 = DIRECTION('ref_axis',(1.,0.,0.)) ;
#11136 = DIRECTION('center_axis',(0.909834542072809,-0.376865806842072,-0.173704547103509)) ;
#11137 = DIRECTION('ref_axis',(0.414971211111278,0.826287510096956,0.38085147315799)) ;
#11138 = DIRECTION('center_axis',(-0.376865806842072,0.909834542072809,0.173704547103509)) ;
#11139 = DIRECTION('ref_axis',(0.926267868185696,0.370179664617618,0.0706742687992893)) ;
#11140 = DIRECTION('center_axis',(0.,0.,1.)) ;
#11141 = DIRECTION('ref_axis',(1.,0.,0.)) ;
#11142 = DIRECTION('center_axis',(0.376865806842072,-0.909834542072809,-0.173704547103509)) ;
#11143 = DIRECTION('ref_axis',(0.926267868185696,0.370179664617618,0.0706742687992893)) ;
#11144 = DIRECTION('center_axis',(0.376865806842073,0.909834542072809,0.173704547103509)) ;
#11145 = DIRECTION('ref_axis',(0.926267868185696,-0.370179664617618,-0.0706742687992894)) ;
#11146 = DIRECTION('center_axis',(0.,0.,1.)) ;
#11147 = DIRECTION('ref_axis',(1.,0.,0.)) ;
#11148 = DIRECTION('center_axis',(-0.376865806842073,-0.909834542072809,-0.173704547103509)) ;
#11149 = DIRECTION('ref_axis',(0.926267868185696,-0.370179664617618,-0.0706742687992894)) ;
#11150 = DIRECTION('center_axis',(0.909834542072809,0.376865806842072,0.173704547103509)) ;
#11151 = DIRECTION('ref_axis',(0.414971211111279,-0.826287510096956,-0.380851473157991)) ;
#11152 = DIRECTION('center_axis',(0.,0.,1.)) ;
#11153 = DIRECTION('ref_axis',(1.,0.,0.)) ;
#11154 = DIRECTION('center_axis',(-0.909834542072809,-0.376865806842072,-0.173704547103509)) ;
#11155 = DIRECTION('ref_axis',(0.414971211111279,-0.826287510096956,-0.380851473157991)) ;
#11156 = DIRECTION('center_axis',(0.90983454207281,-0.376865806842072,0.173704547103509)) ;
#11157 = DIRECTION('ref_axis',(0.414971211111278,0.826287510096956,-0.380851473157991)) ;
#11158 = DIRECTION('center_axis',(0.90983454207281,-0.376865806842072,0.173704547103509)) ;
#11159 = DIRECTION('ref_axis',(0.414971211111278,0.826287510096956,-0.380851473157991)) ;
#11160 = DIRECTION('center_axis',(0.,0.,1.)) ;
#11161 = DIRECTION('ref_axis',(-0.707106781186572,-0.707106781186523,0.)) ;
#11162 = DIRECTION('center_axis',(-0.90983454207281,0.376865806842072,-0.173704547103509)) ;
#11163 = DIRECTION('ref_axis',(0.414971211111278,0.826287510096956,-0.380851473157991)) ;
#11164 = DIRECTION('center_axis',(-0.90983454207281,0.376865806842072,-0.173704547103509)) ;
#11165 = DIRECTION('ref_axis',(0.414971211111278,0.826287510096956,-0.380851473157991)) ;
#11166 = DIRECTION('center_axis',(0.376865806842071,-0.90983454207281,0.173704547103509)) ;
#11167 = DIRECTION('ref_axis',(0.926267868185696,0.370179664617617,-0.0706742687992893)) ;
#11168 = DIRECTION('center_axis',(0.376865806842071,-0.90983454207281,0.173704547103509)) ;
#11169 = DIRECTION('ref_axis',(0.926267868185696,0.370179664617617,-0.0706742687992893)) ;
#11170 = DIRECTION('center_axis',(0.,0.,1.)) ;
#11171 = DIRECTION('ref_axis',(-1.,0.,0.)) ;
#11172 = DIRECTION('center_axis',(-0.376865806842071,0.90983454207281,-0.173704547103509)) ;
#11173 = DIRECTION('ref_axis',(0.926267868185696,0.370179664617617,-0.0706742687992893)) ;
#11174 = DIRECTION('center_axis',(-0.376865806842071,0.90983454207281,-0.173704547103509)) ;
#11175 = DIRECTION('ref_axis',(0.926267868185696,0.370179664617617,-0.0706742687992893)) ;
#11176 = DIRECTION('center_axis',(-0.376865806842072,-0.90983454207281,0.173704547103509)) ;
#11177 = DIRECTION('ref_axis',(0.926267868185696,-0.370179664617617,0.0706742687992892)) ;
#11178 = DIRECTION('center_axis',(-0.376865806842072,-0.90983454207281,0.173704547103509)) ;
#11179 = DIRECTION('ref_axis',(0.926267868185696,-0.370179664617617,0.0706742687992892)) ;
#11180 = DIRECTION('center_axis',(0.,0.,1.)) ;
#11181 = DIRECTION('ref_axis',(-0.707106781186561,0.707106781186534,0.)) ;
#11182 = DIRECTION('center_axis',(0.376865806842072,0.90983454207281,-0.173704547103509)) ;
#11183 = DIRECTION('ref_axis',(0.926267868185696,-0.370179664617617,0.0706742687992892)) ;
#11184 = DIRECTION('center_axis',(0.376865806842072,0.90983454207281,-0.173704547103509)) ;
#11185 = DIRECTION('ref_axis',(0.926267868185696,-0.370179664617617,0.0706742687992892)) ;
#11186 = DIRECTION('center_axis',(-0.90983454207281,-0.376865806842072,0.173704547103509)) ;
#11187 = DIRECTION('ref_axis',(0.414971211111278,-0.826287510096956,0.380851473157991)) ;
#11188 = DIRECTION('center_axis',(-0.90983454207281,-0.376865806842072,0.173704547103509)) ;
#11189 = DIRECTION('ref_axis',(0.414971211111278,-0.826287510096956,0.380851473157991)) ;
#11190 = DIRECTION('center_axis',(0.,0.,1.)) ;
#11191 = DIRECTION('ref_axis',(1.,0.,0.)) ;
#11192 = DIRECTION('center_axis',(0.90983454207281,0.376865806842072,-0.173704547103509)) ;
#11193 = DIRECTION('ref_axis',(0.414971211111278,-0.826287510096956,0.380851473157991)) ;
#11194 = DIRECTION('center_axis',(0.90983454207281,0.376865806842072,-0.173704547103509)) ;
#11195 = DIRECTION('ref_axis',(0.414971211111278,-0.826287510096956,0.380851473157991)) ;
#11196 = DIRECTION('center_axis',(-0.909834542072809,0.376865806842072,0.173704547103509)) ;
#11197 = DIRECTION('ref_axis',(0.414971211111278,0.826287510096956,0.38085147315799)) ;
#11198 = DIRECTION('center_axis',(0.,0.,1.)) ;
#11199 = DIRECTION('ref_axis',(1.,0.,0.)) ;
#11200 = DIRECTION('center_axis',(0.909834542072809,-0.376865806842072,-0.173704547103509)) ;
#11201 = DIRECTION('ref_axis',(0.414971211111278,0.826287510096956,0.38085147315799)) ;
#11202 = DIRECTION('center_axis',(-0.376865806842073,0.909834542072809,0.173704547103509)) ;
#11203 = DIRECTION('ref_axis',(0.926267868185696,0.370179664617618,0.0706742687992896)) ;
#11204 = DIRECTION('center_axis',(0.376865806842073,0.909834542072809,0.173704547103507)) ;
#11205 = DIRECTION('ref_axis',(0.926267868185695,-0.370179664617619,-0.0706742687992891)) ;
#11206 = DIRECTION('center_axis',(0.376865806842073,0.909834542072809,0.173704547103507)) ;
#11207 = DIRECTION('ref_axis',(0.926267868185695,-0.370179664617619,-0.0706742687992891)) ;
#11208 = DIRECTION('',(-0.376865806842074,-0.909834542072809,-0.173704547103507)) ;
#11209 = DIRECTION('center_axis',(-0.694561688421286,-0.694561688421282,-0.187531655873747)) ;
#11210 = DIRECTION('ref_axis',(0.707106781186545,-0.70710678118655,4.46695575243751E-15)) ;
#11211 = DIRECTION('center_axis',(-0.694561688421286,-0.694561688421282,-0.187531655873747)) ;
#11212 = DIRECTION('ref_axis',(0.707106781186545,-0.70710678118655,4.46695575243751E-15)) ;
#11213 = DIRECTION('center_axis',(-0.694561688421286,-0.694561688421282,-0.187531655873747)) ;
#11214 = DIRECTION('ref_axis',(0.707106781186545,-0.70710678118655,4.46695575243751E-15)) ;
#11215 = DIRECTION('center_axis',(0.376865806842073,0.909834542072809,0.173704547103507)) ;
#11216 = DIRECTION('ref_axis',(0.926267868185696,-0.370179664617619,-0.0706742687992891)) ;
#11217 = DIRECTION('center_axis',(0.909834542072811,0.376865806842069,0.17370454710351)) ;
#11218 = DIRECTION('ref_axis',(0.414971211111276,-0.826287510096955,-0.380851473157994)) ;
#11219 = DIRECTION('',(-0.909834542072811,-0.376865806842069,-0.17370454710351)) ;
#11220 = DIRECTION('center_axis',(-0.982258559670136,9.62376035907939E-15,
-0.187531655873751)) ;
#11221 = DIRECTION('ref_axis',(-1.14405485458112E-14,-1.,8.16263856920234E-15)) ;
#11222 = DIRECTION('center_axis',(-0.982258559670136,9.62376035907939E-15,
-0.187531655873751)) ;
#11223 = DIRECTION('ref_axis',(-1.14405485458112E-14,-1.,8.16263856920234E-15)) ;
#11224 = DIRECTION('center_axis',(0.909834542072809,-0.376865806842073,0.173704547103512)) ;
#11225 = DIRECTION('ref_axis',(0.41497121111128,0.826287510096954,-0.380851473157994)) ;
#11226 = DIRECTION('',(-0.909834542072809,0.376865806842073,-0.173704547103512)) ;
#11227 = DIRECTION('center_axis',(-0.694561688421282,0.694561688421288,-0.187531655873744)) ;
#11228 = DIRECTION('ref_axis',(0.707106781186549,0.707106781186546,1.52005041072154E-14)) ;
#11229 = DIRECTION('center_axis',(0.376865806842071,-0.90983454207281,0.173704547103507)) ;
#11230 = DIRECTION('ref_axis',(0.926267868185696,0.370179664617617,-0.0706742687992885)) ;
#11231 = DIRECTION('',(-0.376865806842071,0.90983454207281,-0.173704547103507)) ;
#11232 = DIRECTION('center_axis',(5.58328333024527E-15,0.982258559670136,
-0.187531655873747)) ;
#11233 = DIRECTION('ref_axis',(1.,-5.52745603898742E-15,1.06050028654991E-15)) ;
#11234 = DIRECTION('center_axis',(-0.376865806842073,-0.909834542072809,0.173704547103509)) ;
#11235 = DIRECTION('ref_axis',(0.926267868185696,-0.370179664617619,0.0706742687992895)) ;
#11236 = DIRECTION('',(0.376865806842073,0.909834542072809,-0.173704547103509)) ;
#11237 = DIRECTION('center_axis',(0.694561688421279,0.69456168842129,-0.187531655873747)) ;
#11238 = DIRECTION('ref_axis',(0.707106781186552,-0.707106781186543,-3.03688718421113E-15)) ;
#11239 = DIRECTION('center_axis',(-0.90983454207281,-0.376865806842072,0.173704547103508)) ;
#11240 = DIRECTION('ref_axis',(0.414971211111278,-0.826287510096957,0.38085147315799)) ;
#11241 = DIRECTION('',(0.90983454207281,0.376865806842072,-0.173704547103508)) ;
#11242 = DIRECTION('center_axis',(0.982258559670136,6.5381477562569E-15,-0.187531655873751)) ;
#11243 = DIRECTION('ref_axis',(3.85636467836333E-15,-1.,-1.43970947992231E-14)) ;
#11244 = DIRECTION('center_axis',(0.982258559670136,6.5381477562569E-15,-0.187531655873751)) ;
#11245 = DIRECTION('ref_axis',(3.85636467836333E-15,-1.,-1.43970947992231E-14)) ;
#11246 = DIRECTION('center_axis',(-0.909834542072809,0.376865806842072,0.173704547103511)) ;
#11247 = DIRECTION('ref_axis',(0.414971211111279,0.826287510096954,0.380851473157994)) ;
#11248 = DIRECTION('',(0.909834542072809,-0.376865806842072,-0.173704547103511)) ;
#11249 = DIRECTION('center_axis',(0.69456168842128,-0.694561688421288,-0.187531655873747)) ;
#11250 = DIRECTION('ref_axis',(0.707106781186551,0.707106781186544,-5.65600152826619E-15)) ;
#11251 = DIRECTION('center_axis',(0.69456168842128,-0.694561688421288,-0.187531655873747)) ;
#11252 = DIRECTION('ref_axis',(0.707106781186551,0.707106781186544,-5.65600152826619E-15)) ;
#11253 = DIRECTION('center_axis',(0.69456168842128,-0.694561688421288,-0.187531655873747)) ;
#11254 = DIRECTION('ref_axis',(0.707106781186551,0.707106781186544,-5.65600152826619E-15)) ;
#11255 = DIRECTION('center_axis',(-0.376865806842072,0.909834542072809,0.17370454710351)) ;
#11256 = DIRECTION('ref_axis',(0.926267868185696,0.370179664617617,0.0706742687992896)) ;
#11257 = DIRECTION('',(0.376865806842072,-0.909834542072809,-0.17370454710351)) ;
#11258 = DIRECTION('center_axis',(-4.0404770288341E-15,-0.982258559670136,
-0.187531655873747)) ;
#11259 = DIRECTION('ref_axis',(1.,-3.98491016764209E-15,-7.79307028752587E-16)) ;
#11260 = DIRECTION('center_axis',(-4.0404770288341E-15,-0.982258559670136,
-0.187531655873747)) ;
#11261 = DIRECTION('ref_axis',(1.,-3.98491016764209E-15,-7.79307028752587E-16)) ;
#11262 = DIRECTION('center_axis',(0.376865806842073,0.909834542072809,0.173704547103507)) ;
#11263 = DIRECTION('ref_axis',(0.926267868185695,-0.370179664617619,-0.0706742687992891)) ;
#11264 = DIRECTION('',(-0.376865806842073,-0.909834542072809,-0.173704547103507)) ;
#11265 = DIRECTION('center_axis',(-0.694561688421286,-0.694561688421282,-0.187531655873747)) ;
#11266 = DIRECTION('ref_axis',(0.707106781186545,-0.70710678118655,4.46695575243751E-15)) ;
#11267 = DIRECTION('center_axis',(-0.694561688421286,-0.694561688421282,-0.187531655873747)) ;
#11268 = DIRECTION('ref_axis',(0.707106781186545,-0.70710678118655,4.46695575243751E-15)) ;
#11269 = DIRECTION('center_axis',(-0.694561688421286,-0.694561688421282,-0.187531655873747)) ;
#11270 = DIRECTION('ref_axis',(0.707106781186545,-0.70710678118655,4.46695575243751E-15)) ;
#11271 = DIRECTION('center_axis',(0.909834542072811,0.376865806842069,0.17370454710351)) ;
#11272 = DIRECTION('ref_axis',(0.414971211111276,-0.826287510096955,-0.380851473157994)) ;
#11273 = DIRECTION('',(-0.909834542072811,-0.376865806842069,-0.17370454710351)) ;
#11274 = DIRECTION('center_axis',(-0.982258559670137,6.53814775625699E-15,
-0.187531655873742)) ;
#11275 = DIRECTION('ref_axis',(-4.2259329600398E-15,-1.,-1.29188216725171E-14)) ;
#11276 = DIRECTION('center_axis',(-0.982258559670137,6.53814775625699E-15,
-0.187531655873742)) ;
#11277 = DIRECTION('ref_axis',(-4.2259329600398E-15,-1.,-1.29188216725171E-14)) ;
#11278 = DIRECTION('center_axis',(0.909834542072809,-0.376865806842073,0.173704547103508)) ;
#11279 = DIRECTION('ref_axis',(0.414971211111279,0.826287510096957,-0.380851473157988)) ;
#11280 = DIRECTION('',(-0.909834542072809,0.376865806842073,-0.173704547103508)) ;
#11281 = DIRECTION('center_axis',(-0.694561688421284,0.694561688421284,-0.187531655873748)) ;
#11282 = DIRECTION('ref_axis',(0.707106781186548,0.707106781186547,-3.72781918908455E-15)) ;
#11283 = DIRECTION('center_axis',(0.376865806842071,-0.90983454207281,0.17370454710351)) ;
#11284 = DIRECTION('ref_axis',(0.926267868185696,0.370179664617617,-0.0706742687992895)) ;
#11285 = DIRECTION('',(-0.376865806842071,0.90983454207281,-0.17370454710351)) ;
#11286 = DIRECTION('center_axis',(4.04047702883407E-15,0.982258559670136,
-0.187531655873747)) ;
#11287 = DIRECTION('ref_axis',(1.,-3.98491016764209E-15,7.71272935672663E-16)) ;
#11288 = DIRECTION('center_axis',(-0.376865806842073,-0.909834542072809,0.173704547103508)) ;
#11289 = DIRECTION('ref_axis',(0.926267868185696,-0.370179664617619,0.0706742687992894)) ;
#11290 = DIRECTION('',(0.376865806842073,0.909834542072809,-0.173704547103508)) ;
#11291 = DIRECTION('center_axis',(0.694561688421286,0.694561688421282,-0.187531655873747)) ;
#11292 = DIRECTION('ref_axis',(0.707106781186545,-0.70710678118655,-2.15313694541952E-15)) ;
#11293 = DIRECTION('center_axis',(-0.909834542072809,-0.376865806842072,0.17370454710351)) ;
#11294 = DIRECTION('ref_axis',(0.414971211111279,-0.826287510096955,0.380851473157994)) ;
#11295 = DIRECTION('',(0.909834542072809,0.376865806842072,-0.17370454710351)) ;
#11296 = DIRECTION('center_axis',(0.982258559670136,0.,-0.187531655873751)) ;
#11297 = DIRECTION('ref_axis',(-1.261352613548E-15,-1.,-6.42727446393887E-15)) ;
#11298 = DIRECTION('center_axis',(0.982258559670136,0.,-0.187531655873751)) ;
#11299 = DIRECTION('ref_axis',(-1.261352613548E-15,-1.,-6.42727446393887E-15)) ;
#11300 = DIRECTION('center_axis',(-0.90983454207281,0.376865806842072,0.173704547103509)) ;
#11301 = DIRECTION('ref_axis',(0.414971211111278,0.826287510096956,0.38085147315799)) ;
#11302 = DIRECTION('',(0.90983454207281,-0.376865806842072,-0.173704547103509)) ;
#11303 = DIRECTION('center_axis',(0.694561688421279,-0.69456168842129,-0.187531655873747)) ;
#11304 = DIRECTION('ref_axis',(0.707106781186553,0.707106781186542,-4.4990921247572E-16)) ;
#11305 = DIRECTION('center_axis',(0.694561688421279,-0.69456168842129,-0.187531655873747)) ;
#11306 = DIRECTION('ref_axis',(0.707106781186553,0.707106781186542,-4.4990921247572E-16)) ;
#11307 = DIRECTION('center_axis',(0.694561688421279,-0.69456168842129,-0.187531655873747)) ;
#11308 = DIRECTION('ref_axis',(0.707106781186553,0.707106781186542,-4.4990921247572E-16)) ;
#11309 = DIRECTION('center_axis',(-0.376865806842072,0.909834542072809,0.173704547103509)) ;
#11310 = DIRECTION('ref_axis',(0.926267868185696,0.370179664617618,0.0706742687992892)) ;
#11311 = DIRECTION('',(0.376865806842072,-0.909834542072809,-0.173704547103509)) ;
#11312 = DIRECTION('center_axis',(0.,-0.982258559670136,-0.187531655873747)) ;
#11313 = DIRECTION('ref_axis',(1.,0.,-8.03409307992359E-18)) ;
#11314 = DIRECTION('center_axis',(0.,-0.982258559670136,-0.187531655873747)) ;
#11315 = DIRECTION('ref_axis',(1.,0.,-8.03409307992359E-18)) ;
#11316 = DIRECTION('center_axis',(0.376865806842073,0.909834542072809,0.173704547103509)) ;
#11317 = DIRECTION('ref_axis',(0.926267868185696,-0.370179664617619,-0.0706742687992895)) ;
#11318 = DIRECTION('',(-0.376865806842073,-0.909834542072809,-0.173704547103509)) ;
#11319 = DIRECTION('center_axis',(-0.69456168842128,-0.694561688421288,-0.187531655873749)) ;
#11320 = DIRECTION('ref_axis',(0.707106781186551,-0.707106781186544,6.71650181481614E-15)) ;
#11321 = DIRECTION('center_axis',(-0.69456168842128,-0.694561688421288,-0.187531655873749)) ;
#11322 = DIRECTION('ref_axis',(0.707106781186551,-0.707106781186544,6.71650181481614E-15)) ;
#11323 = DIRECTION('center_axis',(-0.69456168842128,-0.694561688421288,-0.187531655873749)) ;
#11324 = DIRECTION('ref_axis',(0.707106781186551,-0.707106781186544,6.71650181481614E-15)) ;
#11325 = DIRECTION('center_axis',(0.90983454207281,0.37686580684207,0.173704547103509)) ;
#11326 = DIRECTION('ref_axis',(0.414971211111277,-0.826287510096957,-0.380851473157992)) ;
#11327 = DIRECTION('',(-0.90983454207281,-0.37686580684207,-0.173704547103509)) ;
#11328 = DIRECTION('center_axis',(-0.982258559670136,0.,-0.187531655873751)) ;
#11329 = DIRECTION('ref_axis',(-2.45843248245662E-15,-1.,1.2726003438599E-14)) ;
#11330 = DIRECTION('center_axis',(-0.982258559670136,0.,-0.187531655873751)) ;
#11331 = DIRECTION('ref_axis',(-2.45843248245662E-15,-1.,1.2726003438599E-14)) ;
#11332 = DIRECTION('center_axis',(0.909834542072809,-0.376865806842073,0.17370454710351)) ;
#11333 = DIRECTION('ref_axis',(0.41497121111128,0.826287510096955,-0.380851473157992)) ;
#11334 = DIRECTION('',(-0.909834542072809,0.376865806842073,-0.17370454710351)) ;
#11335 = DIRECTION('center_axis',(-0.694561688421284,0.694561688421284,-0.187531655873747)) ;
#11336 = DIRECTION('ref_axis',(0.707106781186547,0.707106781186548,2.73159164717402E-15)) ;
#11337 = DIRECTION('center_axis',(0.376865806842071,-0.90983454207281,0.173704547103509)) ;
#11338 = DIRECTION('ref_axis',(0.926267868185696,0.370179664617617,-0.070674268799289)) ;
#11339 = DIRECTION('',(-0.376865806842071,0.90983454207281,-0.173704547103509)) ;
#11340 = DIRECTION('center_axis',(6.53814775625694E-15,0.982258559670136,
-0.187531655873747)) ;
#11341 = DIRECTION('ref_axis',(1.,-6.42727446393886E-15,1.22118214814838E-15)) ;
#11342 = DIRECTION('center_axis',(-0.376865806842073,-0.909834542072809,0.17370454710351)) ;
#11343 = DIRECTION('ref_axis',(0.926267868185696,-0.370179664617618,0.0706742687992898)) ;
#11344 = DIRECTION('',(0.376865806842073,0.909834542072809,-0.17370454710351)) ;
#11345 = DIRECTION('center_axis',(0.694561688421283,0.694561688421285,-0.18753165587375)) ;
#11346 = DIRECTION('ref_axis',(0.707106781186548,-0.707106781186547,-7.26282014425093E-15)) ;
#11347 = DIRECTION('center_axis',(-0.90983454207281,-0.376865806842071,0.173704547103508)) ;
#11348 = DIRECTION('ref_axis',(0.414971211111277,-0.826287510096957,0.38085147315799)) ;
#11349 = DIRECTION('',(0.90983454207281,0.376865806842071,-0.173704547103508)) ;
#11350 = DIRECTION('center_axis',(0.982258559670137,-8.08095405766815E-15,
-0.187531655873742)) ;
#11351 = DIRECTION('ref_axis',(-6.29069488158015E-15,-1.,9.89800267446583E-15)) ;
#11352 = DIRECTION('center_axis',(0.982258559670137,-8.08095405766815E-15,
-0.187531655873742)) ;
#11353 = DIRECTION('ref_axis',(-6.29069488158015E-15,-1.,9.89800267446583E-15)) ;
#11354 = DIRECTION('center_axis',(-0.909834542072809,0.376865806842072,0.17370454710351)) ;
#11355 = DIRECTION('ref_axis',(0.414971211111279,0.826287510096955,0.380851473157992)) ;
#11356 = DIRECTION('',(0.909834542072809,-0.376865806842072,-0.17370454710351)) ;
#11357 = DIRECTION('center_axis',(0.694561688421279,-0.694561688421289,-0.187531655873747)) ;
#11358 = DIRECTION('ref_axis',(0.707106781186552,0.707106781186543,-3.3743190935679E-15)) ;
#11359 = DIRECTION('center_axis',(0.694561688421279,-0.694561688421289,-0.187531655873747)) ;
#11360 = DIRECTION('ref_axis',(0.707106781186552,0.707106781186543,-3.3743190935679E-15)) ;
#11361 = DIRECTION('center_axis',(0.694561688421279,-0.694561688421289,-0.187531655873747)) ;
#11362 = DIRECTION('ref_axis',(0.707106781186552,0.707106781186543,-3.3743190935679E-15)) ;
#11363 = DIRECTION('center_axis',(-0.376865806842072,0.909834542072809,0.173704547103509)) ;
#11364 = DIRECTION('ref_axis',(0.926267868185696,0.370179664617618,0.0706742687992893)) ;
#11365 = DIRECTION('',(0.376865806842072,-0.909834542072809,-0.173704547103509)) ;
#11366 = DIRECTION('center_axis',(-1.5428063014112E-15,-0.982258559670136,
-0.187531655873747)) ;
#11367 = DIRECTION('ref_axis',(1.,-1.54254587134533E-15,-3.1332963011702E-16)) ;
#11368 = DIRECTION('center_axis',(-1.5428063014112E-15,-0.982258559670136,
-0.187531655873747)) ;
#11369 = DIRECTION('ref_axis',(1.,-1.54254587134533E-15,-3.1332963011702E-16)) ;
#11370 = DIRECTION('center_axis',(0.376865806842073,0.909834542072809,0.17370454710351)) ;
#11371 = DIRECTION('ref_axis',(0.926267868185696,-0.370179664617619,-0.0706742687992899)) ;
#11372 = DIRECTION('',(-0.376865806842073,-0.909834542072809,-0.17370454710351)) ;
#11373 = DIRECTION('center_axis',(-0.694561688421283,-0.694561688421286,-0.187531655873747)) ;
#11374 = DIRECTION('ref_axis',(0.707106781186549,-0.707106781186546,-5.62386515594652E-16)) ;
#11375 = DIRECTION('center_axis',(-0.694561688421283,-0.694561688421286,-0.187531655873747)) ;
#11376 = DIRECTION('ref_axis',(0.707106781186549,-0.707106781186546,-5.62386515594652E-16)) ;
#11377 = DIRECTION('center_axis',(-0.694561688421283,-0.694561688421286,-0.187531655873747)) ;
#11378 = DIRECTION('ref_axis',(0.707106781186549,-0.707106781186546,-5.62386515594652E-16)) ;
#11379 = DIRECTION('center_axis',(0.90983454207281,0.376865806842072,0.173704547103509)) ;
#11380 = DIRECTION('ref_axis',(0.414971211111278,-0.826287510096956,-0.380851473157991)) ;
#11381 = DIRECTION('',(-0.90983454207281,-0.376865806842072,-0.173704547103509)) ;
#11382 = DIRECTION('center_axis',(-0.982258559670137,0.,-0.187531655873742)) ;
#11383 = DIRECTION('ref_axis',(2.10493238693998E-15,-1.,-1.10549120779749E-14)) ;
#11384 = DIRECTION('center_axis',(-0.982258559670137,0.,-0.187531655873742)) ;
#11385 = DIRECTION('ref_axis',(2.10493238693998E-15,-1.,-1.10549120779749E-14)) ;
#11386 = DIRECTION('center_axis',(0.90983454207281,-0.376865806842072,0.173704547103508)) ;
#11387 = DIRECTION('ref_axis',(0.414971211111278,0.826287510096957,-0.380851473157989)) ;
#11388 = DIRECTION('',(-0.90983454207281,0.376865806842072,-0.173704547103508)) ;
#11389 = DIRECTION('center_axis',(-0.694561688421283,0.694561688421285,-0.187531655873748)) ;
#11390 = DIRECTION('ref_axis',(0.707106781186549,0.707106781186546,-3.9849101676421E-15)) ;
#11391 = DIRECTION('center_axis',(0.376865806842071,-0.90983454207281,0.173704547103509)) ;
#11392 = DIRECTION('ref_axis',(0.926267868185696,0.370179664617617,-0.0706742687992893)) ;
#11393 = DIRECTION('',(-0.376865806842071,0.90983454207281,-0.173704547103509)) ;
#11394 = DIRECTION('center_axis',(4.04047702883407E-15,0.982258559670136,
-0.187531655873749)) ;
#11395 = DIRECTION('ref_axis',(1.,-3.98491016764209E-15,7.6323884259274E-16)) ;
#11396 = DIRECTION('center_axis',(-0.376865806842073,-0.909834542072809,0.173704547103509)) ;
#11397 = DIRECTION('ref_axis',(0.926267868185696,-0.370179664617619,0.0706742687992897)) ;
#11398 = DIRECTION('',(0.376865806842073,0.909834542072809,-0.173704547103509)) ;
#11399 = DIRECTION('center_axis',(0.694561688421284,0.694561688421285,-0.187531655873748)) ;
#11400 = DIRECTION('ref_axis',(0.707106781186548,-0.707106781186547,-2.8601371364528E-15)) ;
#11401 = DIRECTION('center_axis',(-0.90983454207281,-0.376865806842072,0.17370454710351)) ;
#11402 = DIRECTION('ref_axis',(0.414971211111278,-0.826287510096955,0.380851473157992)) ;
#11403 = DIRECTION('',(0.909834542072809,0.376865806842072,-0.17370454710351)) ;
#11404 = DIRECTION('center_axis',(0.982258559670137,0.,-0.187531655873743)) ;
#11405 = DIRECTION('ref_axis',(1.94425052534151E-15,-1.,1.05407301208597E-14)) ;
#11406 = DIRECTION('center_axis',(0.982258559670137,0.,-0.187531655873743)) ;
#11407 = DIRECTION('ref_axis',(1.94425052534151E-15,-1.,1.05407301208597E-14)) ;
#11408 = DIRECTION('center_axis',(-0.909834542072809,0.376865806842072,0.173704547103509)) ;
#11409 = DIRECTION('ref_axis',(0.414971211111278,0.826287510096956,0.38085147315799)) ;
#11410 = DIRECTION('',(0.909834542072809,-0.376865806842072,-0.173704547103509)) ;
#11411 = DIRECTION('center_axis',(0.69456168842128,-0.694561688421288,-0.187531655873748)) ;
#11412 = DIRECTION('ref_axis',(0.707106781186552,0.707106781186543,1.83177322222257E-15)) ;
#11413 = DIRECTION('center_axis',(0.69456168842128,-0.694561688421288,-0.187531655873748)) ;
#11414 = DIRECTION('ref_axis',(0.707106781186552,0.707106781186543,1.83177322222257E-15)) ;
#11415 = DIRECTION('center_axis',(0.69456168842128,-0.694561688421288,-0.187531655873748)) ;
#11416 = DIRECTION('ref_axis',(0.707106781186552,0.707106781186543,1.83177322222257E-15)) ;
#11417 = DIRECTION('center_axis',(-0.376865806842072,0.909834542072809,0.173704547103509)) ;
#11418 = DIRECTION('ref_axis',(0.926267868185696,0.370179664617618,0.0706742687992893)) ;
#11419 = DIRECTION('',(0.376865806842072,-0.909834542072809,-0.173704547103509)) ;
#11420 = DIRECTION('center_axis',(-7.71403150705611E-16,-0.982258559670136,
-0.187531655873747)) ;
#11421 = DIRECTION('ref_axis',(1.,-8.35545680312053E-16,-1.76750047758319E-16)) ;
#11422 = DIRECTION('center_axis',(-7.71403150705611E-16,-0.982258559670136,
-0.187531655873747)) ;
#11423 = DIRECTION('ref_axis',(1.,-8.35545680312053E-16,-1.76750047758319E-16)) ;
#11424 = DIRECTION('center_axis',(0.376865806842073,0.909834542072809,0.173704547103509)) ;
#11425 = DIRECTION('ref_axis',(0.926267868185696,-0.370179664617618,-0.0706742687992894)) ;
#11426 = DIRECTION('',(-0.376865806842073,-0.909834542072809,-0.173704547103509)) ;
#11427 = DIRECTION('center_axis',(-0.694561688421285,-0.694561688421283,-0.187531655873748)) ;
#11428 = DIRECTION('ref_axis',(0.707106781186546,-0.707106781186549,3.31004634892852E-15)) ;
#11429 = DIRECTION('center_axis',(-0.694561688421285,-0.694561688421283,-0.187531655873748)) ;
#11430 = DIRECTION('ref_axis',(0.707106781186546,-0.707106781186549,3.31004634892852E-15)) ;
#11431 = DIRECTION('center_axis',(-0.694561688421285,-0.694561688421283,-0.187531655873748)) ;
#11432 = DIRECTION('ref_axis',(0.707106781186546,-0.707106781186549,3.31004634892852E-15)) ;
#11433 = DIRECTION('center_axis',(0.909834542072809,0.376865806842072,0.173704547103509)) ;
#11434 = DIRECTION('ref_axis',(0.414971211111279,-0.826287510096956,-0.380851473157991)) ;
#11435 = DIRECTION('',(-0.909834542072809,-0.376865806842072,-0.173704547103509)) ;
#11436 = DIRECTION('center_axis',(-0.982258559670137,0.,-0.187531655873743)) ;
#11437 = DIRECTION('ref_axis',(1.82373912914265E-15,-1.,-9.70518444054769E-15)) ;
#11438 = DIRECTION('center_axis',(-0.982258559670137,0.,-0.187531655873743)) ;
#11439 = DIRECTION('ref_axis',(1.82373912914265E-15,-1.,-9.70518444054769E-15)) ;
#11440 = DIRECTION('center_axis',(0.90983454207281,-0.376865806842072,0.173704547103509)) ;
#11441 = DIRECTION('ref_axis',(0.414971211111278,0.826287510096956,-0.380851473157991)) ;
#11442 = DIRECTION('',(-0.90983454207281,0.376865806842072,-0.173704547103509)) ;
#11443 = DIRECTION('center_axis',(-0.694561688421285,0.694561688421283,-0.18753165587375)) ;
#11444 = DIRECTION('ref_axis',(0.707106781186547,0.707106781186548,-6.10591074074193E-15)) ;
#11445 = DIRECTION('center_axis',(0.376865806842071,-0.90983454207281,0.173704547103509)) ;
#11446 = DIRECTION('ref_axis',(0.926267868185696,0.370179664617617,-0.0706742687992893)) ;
#11447 = DIRECTION('',(-0.376865806842071,0.90983454207281,-0.173704547103509)) ;
#11448 = DIRECTION('center_axis',(4.81188017953967E-15,0.982258559670136,
-0.187531655873747)) ;
#11449 = DIRECTION('ref_axis',(1.,-4.75618310331476E-15,9.15886611111287E-16)) ;
#11450 = DIRECTION('center_axis',(-0.376865806842072,-0.90983454207281,0.173704547103509)) ;
#11451 = DIRECTION('ref_axis',(0.926267868185696,-0.370179664617617,0.0706742687992892)) ;
#11452 = DIRECTION('',(0.376865806842072,0.90983454207281,-0.173704547103509)) ;
#11453 = DIRECTION('center_axis',(0.694561688421281,0.694561688421287,-0.187531655873748)) ;
#11454 = DIRECTION('ref_axis',(0.70710678118655,-0.707106781186545,-3.90456923684287E-15)) ;
#11455 = DIRECTION('center_axis',(-0.90983454207281,-0.376865806842072,0.173704547103509)) ;
#11456 = DIRECTION('ref_axis',(0.414971211111278,-0.826287510096956,0.380851473157991)) ;
#11457 = DIRECTION('',(0.909834542072809,0.376865806842072,-0.173704547103509)) ;
#11458 = DIRECTION('center_axis',(0.982258559670137,-8.85235720837373E-15,
-0.187531655873743)) ;
#11459 = DIRECTION('ref_axis',(-6.81291093177518E-15,-1.,1.11834575672536E-14)) ;
#11460 = DIRECTION('center_axis',(0.982258559670137,-8.85235720837373E-15,
-0.187531655873743)) ;
#11461 = DIRECTION('ref_axis',(-6.81291093177518E-15,-1.,1.11834575672536E-14)) ;
#11462 = DIRECTION('center_axis',(-0.909834542072809,0.376865806842072,0.173704547103509)) ;
#11463 = DIRECTION('ref_axis',(0.414971211111278,0.826287510096956,0.38085147315799)) ;
#11464 = DIRECTION('',(0.909834542072809,-0.376865806842072,-0.173704547103509)) ;
#11465 = DIRECTION('center_axis',(0.694561688421281,-0.694561688421288,-0.187531655873748)) ;
#11466 = DIRECTION('ref_axis',(0.707106781186551,0.707106781186544,2.18527331773921E-15)) ;
#11467 = DIRECTION('center_axis',(0.694561688421281,-0.694561688421288,-0.187531655873748)) ;
#11468 = DIRECTION('ref_axis',(0.707106781186551,0.707106781186544,2.18527331773921E-15)) ;
#11469 = DIRECTION('center_axis',(0.694561688421281,-0.694561688421288,-0.187531655873748)) ;
#11470 = DIRECTION('ref_axis',(0.707106781186551,0.707106781186544,2.18527331773921E-15)) ;
#11471 = DIRECTION('center_axis',(-0.376865806842073,0.909834542072809,0.173704547103509)) ;
#11472 = DIRECTION('ref_axis',(0.926267868185696,0.370179664617618,0.0706742687992896)) ;
#11473 = DIRECTION('',(0.376865806842073,-0.909834542072809,-0.173704547103509)) ;
#11474 = DIRECTION('center_axis',(0.376865806842073,-0.909834542072809,-0.173704547103509)) ;
#11475 = DIRECTION('ref_axis',(0.926267868185696,0.370179664617618,0.0706742687992896)) ;
#11476 = DIRECTION('center_axis',(0.376865806842073,-0.909834542072809,-0.173704547103509)) ;
#11477 = DIRECTION('ref_axis',(-0.926267868185696,-0.370179664617618,-0.0706742687992896)) ;
#11478 = DIRECTION('axis',(0.,0.,1.)) ;
#11479 = DIRECTION('refdir',(1.,0.,0.)) ;
#11480 = DIRECTION('center_axis',(0.,0.,-1.)) ;
#11481 = DIRECTION('ref_axis',(-1.,0.,0.)) ;
#11482 = DIRECTION('center_axis',(0.,0.,-1.)) ;
#11483 = DIRECTION('ref_axis',(1.,0.,0.)) ;
#11484 = DIRECTION('center_axis',(0.,0.,-1.)) ;
#11485 = DIRECTION('ref_axis',(1.,0.,0.)) ;
#11486 = DIRECTION('center_axis',(0.,0.,1.)) ;
#11487 = DIRECTION('ref_axis',(1.,0.,0.)) ;
#11488 = DIRECTION('center_axis',(0.,0.,1.)) ;
#11489 = DIRECTION('ref_axis',(1.,0.,0.)) ;
#11490 = DIRECTION('center_axis',(0.,0.,1.)) ;
#11491 = DIRECTION('ref_axis',(1.,0.,0.)) ;
#11492 = DIRECTION('center_axis',(0.,0.,1.)) ;
#11493 = DIRECTION('ref_axis',(1.,0.,0.)) ;
#11494 = DIRECTION('',(0.,0.,-1.)) ;
#11495 = DIRECTION('center_axis',(0.,0.,1.)) ;
#11496 = DIRECTION('ref_axis',(1.,0.,0.)) ;
#11497 = DIRECTION('center_axis',(0.,0.,1.)) ;
#11498 = DIRECTION('ref_axis',(1.,0.,0.)) ;
#11499 = DIRECTION('',(0.,0.,-1.)) ;
#11500 = DIRECTION('center_axis',(0.,0.,1.)) ;
#11501 = DIRECTION('ref_axis',(1.,0.,0.)) ;
#11502 = DIRECTION('',(0.,0.,-1.)) ;
#11503 = DIRECTION('center_axis',(0.,0.,-1.)) ;
#11504 = DIRECTION('ref_axis',(1.,0.,0.)) ;
#11505 = DIRECTION('center_axis',(0.,0.,-1.)) ;
#11506 = DIRECTION('ref_axis',(-1.,0.,0.)) ;
#11507 = DIRECTION('center_axis',(0.,0.,1.)) ;
#11508 = DIRECTION('ref_axis',(1.,0.,0.)) ;
#11509 = DIRECTION('axis',(0.,0.,1.)) ;
#11510 = DIRECTION('refdir',(1.,0.,0.)) ;
#11511 = DIRECTION('center_axis',(0.,0.,1.)) ;
#11512 = DIRECTION('ref_axis',(1.,0.,0.)) ;
#11513 = DIRECTION('',(0.,1.,0.)) ;
#11514 = DIRECTION('',(-1.,0.,0.)) ;
#11515 = DIRECTION('',(0.,-1.,0.)) ;
#11516 = DIRECTION('',(1.,0.,0.)) ;
#11517 = DIRECTION('center_axis',(0.,1.,0.)) ;
#11518 = DIRECTION('ref_axis',(0.,0.,1.)) ;
#11519 = DIRECTION('',(0.,0.,-1.)) ;
#11520 = DIRECTION('',(-1.,0.,0.)) ;
#11521 = DIRECTION('',(0.,0.,-1.)) ;
#11522 = DIRECTION('center_axis',(1.,0.,0.)) ;
#11523 = DIRECTION('ref_axis',(0.,0.,-1.)) ;
#11524 = DIRECTION('',(0.,0.,-1.)) ;
#11525 = DIRECTION('',(0.,1.,0.)) ;
#11526 = DIRECTION('center_axis',(0.,-1.,0.)) ;
#11527 = DIRECTION('ref_axis',(0.,0.,-1.)) ;
#11528 = DIRECTION('',(0.,0.,-1.)) ;
#11529 = DIRECTION('',(1.,0.,0.)) ;
#11530 = DIRECTION('center_axis',(-1.,0.,0.)) ;
#11531 = DIRECTION('ref_axis',(0.,0.,1.)) ;
#11532 = DIRECTION('',(0.,-1.,0.)) ;
#11533 = DIRECTION('center_axis',(0.,0.,1.)) ;
#11534 = DIRECTION('ref_axis',(1.,0.,0.)) ;
#11535 = DIRECTION('center_axis',(0.,0.,1.)) ;
#11536 = DIRECTION('ref_axis',(1.,0.,0.)) ;
#11537 = DIRECTION('',(0.,0.,1.)) ;
#11538 = DIRECTION('center_axis',(0.,0.,1.)) ;
#11539 = DIRECTION('ref_axis',(1.,0.,0.)) ;
#11540 = DIRECTION('center_axis',(0.,0.,1.)) ;
#11541 = DIRECTION('ref_axis',(1.,0.,0.)) ;
#11542 = DIRECTION('center_axis',(0.,0.,1.)) ;
#11543 = DIRECTION('ref_axis',(1.,0.,0.)) ;
#11544 = DIRECTION('',(0.,1.,0.)) ;
#11545 = DIRECTION('',(-1.,0.,0.)) ;
#11546 = DIRECTION('',(0.,-1.,0.)) ;
#11547 = DIRECTION('',(1.,0.,0.)) ;
#11548 = DIRECTION('center_axis',(0.,0.,1.)) ;
#11549 = DIRECTION('ref_axis',(1.,0.,0.)) ;
#11550 = DIRECTION('',(0.,-1.,0.)) ;
#11551 = DIRECTION('',(-1.,0.,0.)) ;
#11552 = DIRECTION('',(0.,1.,0.)) ;
#11553 = DIRECTION('',(1.,0.,0.)) ;
#11554 = DIRECTION('center_axis',(0.,1.,0.)) ;
#11555 = DIRECTION('ref_axis',(0.,0.,1.)) ;
#11556 = DIRECTION('',(0.,0.,-1.)) ;
#11557 = DIRECTION('',(0.,0.,-1.)) ;
#11558 = DIRECTION('center_axis',(1.,0.,0.)) ;
#11559 = DIRECTION('ref_axis',(0.,0.,-1.)) ;
#11560 = DIRECTION('',(0.,0.,-1.)) ;
#11561 = DIRECTION('center_axis',(0.,-1.,0.)) ;
#11562 = DIRECTION('ref_axis',(0.,0.,-1.)) ;
#11563 = DIRECTION('',(0.,0.,-1.)) ;
#11564 = DIRECTION('center_axis',(-1.,0.,0.)) ;
#11565 = DIRECTION('ref_axis',(0.,0.,1.)) ;
#11566 = DIRECTION('axis',(0.,0.,1.)) ;
#11567 = DIRECTION('refdir',(1.,0.,0.)) ;
#11568 = DIRECTION('center_axis',(0.,0.,1.)) ;
#11569 = DIRECTION('ref_axis',(1.,0.,0.)) ;
#11570 = DIRECTION('center_axis',(-0.381576765574098,-0.921207802535445,-0.0759957664730569)) ;
#11571 = DIRECTION('ref_axis',(0.924337152760836,-0.38028493462931,-0.0313719065402714)) ;
#11572 = DIRECTION('center_axis',(0.921207802535446,0.381576765574096,0.0759957664730549)) ;
#11573 = DIRECTION('ref_axis',(0.389070924829671,-0.90346379356664,-0.179936069664646)) ;
#11574 = DIRECTION('center_axis',(0.,0.,1.)) ;
#11575 = DIRECTION('ref_axis',(1.,0.,0.)) ;
#11576 = DIRECTION('center_axis',(-0.921207802535446,-0.381576765574096,-0.0759957664730549)) ;
#11577 = DIRECTION('ref_axis',(0.389070924829671,-0.90346379356664,-0.179936069664646)) ;
#11578 = DIRECTION('center_axis',(0.921207802535444,-0.381576765574099,0.075995766473057)) ;
#11579 = DIRECTION('ref_axis',(0.389070924829674,0.903463793566638,-0.179936069664649)) ;
#11580 = DIRECTION('center_axis',(0.921207802535444,-0.381576765574099,0.075995766473057)) ;
#11581 = DIRECTION('ref_axis',(0.389070924829674,0.903463793566638,-0.179936069664649)) ;
#11582 = DIRECTION('center_axis',(0.,0.,1.)) ;
#11583 = DIRECTION('ref_axis',(-0.707106781186494,-0.707106781186601,0.)) ;
#11584 = DIRECTION('center_axis',(-0.921207802535444,0.381576765574099,-0.075995766473057)) ;
#11585 = DIRECTION('ref_axis',(0.389070924829674,0.903463793566638,-0.179936069664649)) ;
#11586 = DIRECTION('center_axis',(-0.921207802535444,0.381576765574099,-0.075995766473057)) ;
#11587 = DIRECTION('ref_axis',(0.389070924829674,0.903463793566638,-0.179936069664649)) ;
#11588 = DIRECTION('center_axis',(0.381576765574096,-0.921207802535445,0.0759957664730569)) ;
#11589 = DIRECTION('ref_axis',(0.924337152760837,0.380284934629308,-0.0313719065402712)) ;
#11590 = DIRECTION('center_axis',(0.381576765574096,-0.921207802535445,0.0759957664730569)) ;
#11591 = DIRECTION('ref_axis',(0.924337152760837,0.380284934629308,-0.0313719065402712)) ;
#11592 = DIRECTION('center_axis',(0.,0.,1.)) ;
#11593 = DIRECTION('ref_axis',(-1.,0.,0.)) ;
#11594 = DIRECTION('center_axis',(-0.381576765574096,0.921207802535445,-0.0759957664730569)) ;
#11595 = DIRECTION('ref_axis',(0.924337152760837,0.380284934629308,-0.0313719065402712)) ;
#11596 = DIRECTION('center_axis',(-0.381576765574096,0.921207802535445,-0.0759957664730569)) ;
#11597 = DIRECTION('ref_axis',(0.924337152760837,0.380284934629308,-0.0313719065402712)) ;
#11598 = DIRECTION('center_axis',(-0.3815767655741,-0.921207802535444,0.0759957664730569)) ;
#11599 = DIRECTION('ref_axis',(0.924337152760836,-0.380284934629312,0.0313719065402716)) ;
#11600 = DIRECTION('center_axis',(-0.3815767655741,-0.921207802535444,0.0759957664730569)) ;
#11601 = DIRECTION('ref_axis',(0.924337152760836,-0.380284934629312,0.0313719065402716)) ;
#11602 = DIRECTION('center_axis',(0.,0.,1.)) ;
#11603 = DIRECTION('ref_axis',(-0.707106781186548,0.707106781186548,0.)) ;
#11604 = DIRECTION('center_axis',(0.3815767655741,0.921207802535444,-0.0759957664730569)) ;
#11605 = DIRECTION('ref_axis',(0.924337152760836,-0.380284934629312,0.0313719065402716)) ;
#11606 = DIRECTION('center_axis',(0.3815767655741,0.921207802535444,-0.0759957664730569)) ;
#11607 = DIRECTION('ref_axis',(0.924337152760836,-0.380284934629312,0.0313719065402716)) ;
#11608 = DIRECTION('center_axis',(-0.921207802535445,-0.381576765574097,0.0759957664730571)) ;
#11609 = DIRECTION('ref_axis',(0.389070924829673,-0.903463793566638,0.17993606966465)) ;
#11610 = DIRECTION('center_axis',(-0.921207802535445,-0.381576765574097,0.0759957664730571)) ;
#11611 = DIRECTION('ref_axis',(0.389070924829673,-0.903463793566638,0.17993606966465)) ;
#11612 = DIRECTION('center_axis',(0.,0.,1.)) ;
#11613 = DIRECTION('ref_axis',(1.,0.,0.)) ;
#11614 = DIRECTION('center_axis',(0.921207802535445,0.381576765574097,-0.0759957664730571)) ;
#11615 = DIRECTION('ref_axis',(0.389070924829673,-0.903463793566638,0.17993606966465)) ;
#11616 = DIRECTION('center_axis',(0.921207802535445,0.381576765574097,-0.0759957664730571)) ;
#11617 = DIRECTION('ref_axis',(0.389070924829673,-0.903463793566638,0.17993606966465)) ;
#11618 = DIRECTION('center_axis',(-0.921207802535444,0.381576765574099,0.075995766473057)) ;
#11619 = DIRECTION('ref_axis',(0.389070924829674,0.903463793566638,0.179936069664649)) ;
#11620 = DIRECTION('center_axis',(0.,0.,1.)) ;
#11621 = DIRECTION('ref_axis',(1.,0.,0.)) ;
#11622 = DIRECTION('center_axis',(0.921207802535444,-0.381576765574099,-0.075995766473057)) ;
#11623 = DIRECTION('ref_axis',(0.389070924829674,0.903463793566638,0.179936069664649)) ;
#11624 = DIRECTION('center_axis',(-0.381576765574098,0.921207802535444,0.075995766473057)) ;
#11625 = DIRECTION('ref_axis',(0.924337152760836,0.380284934629311,0.0313719065402715)) ;
#11626 = DIRECTION('center_axis',(0.,0.,1.)) ;
#11627 = DIRECTION('ref_axis',(1.,0.,0.)) ;
#11628 = DIRECTION('center_axis',(0.381576765574098,-0.921207802535444,-0.075995766473057)) ;
#11629 = DIRECTION('ref_axis',(0.924337152760836,0.380284934629311,0.0313719065402715)) ;
#11630 = DIRECTION('center_axis',(0.381576765574098,0.921207802535445,0.0759957664730568)) ;
#11631 = DIRECTION('ref_axis',(0.924337152760837,-0.38028493462931,-0.0313719065402713)) ;
#11632 = DIRECTION('center_axis',(0.,0.,1.)) ;
#11633 = DIRECTION('ref_axis',(1.,0.,0.)) ;
#11634 = DIRECTION('center_axis',(-0.381576765574098,-0.921207802535445,-0.0759957664730568)) ;
#11635 = DIRECTION('ref_axis',(0.924337152760837,-0.38028493462931,-0.0313719065402713)) ;
#11636 = DIRECTION('center_axis',(0.921207802535445,0.381576765574097,0.0759957664730571)) ;
#11637 = DIRECTION('ref_axis',(0.389070924829673,-0.903463793566638,-0.17993606966465)) ;
#11638 = DIRECTION('center_axis',(0.,0.,1.)) ;
#11639 = DIRECTION('ref_axis',(1.,0.,0.)) ;
#11640 = DIRECTION('center_axis',(-0.921207802535445,-0.381576765574097,-0.0759957664730571)) ;
#11641 = DIRECTION('ref_axis',(0.389070924829673,-0.903463793566638,-0.17993606966465)) ;
#11642 = DIRECTION('center_axis',(0.921207802535445,-0.381576765574097,0.0759957664730568)) ;
#11643 = DIRECTION('ref_axis',(0.389070924829672,0.903463793566639,-0.179936069664649)) ;
#11644 = DIRECTION('center_axis',(0.921207802535445,-0.381576765574097,0.0759957664730568)) ;
#11645 = DIRECTION('ref_axis',(0.389070924829672,0.903463793566639,-0.179936069664649)) ;
#11646 = DIRECTION('center_axis',(0.,0.,1.)) ;
#11647 = DIRECTION('ref_axis',(-0.707106781186525,-0.70710678118657,0.)) ;
#11648 = DIRECTION('center_axis',(-0.921207802535445,0.381576765574097,-0.0759957664730568)) ;
#11649 = DIRECTION('ref_axis',(0.389070924829672,0.903463793566639,-0.179936069664649)) ;
#11650 = DIRECTION('center_axis',(-0.921207802535445,0.381576765574097,-0.0759957664730568)) ;
#11651 = DIRECTION('ref_axis',(0.389070924829672,0.903463793566639,-0.179936069664649)) ;
#11652 = DIRECTION('center_axis',(0.381576765574097,-0.921207802535445,0.075995766473055)) ;
#11653 = DIRECTION('ref_axis',(0.924337152760837,0.380284934629309,-0.0313719065402705)) ;
#11654 = DIRECTION('center_axis',(0.381576765574097,-0.921207802535445,0.075995766473055)) ;
#11655 = DIRECTION('ref_axis',(0.924337152760837,0.380284934629309,-0.0313719065402705)) ;
#11656 = DIRECTION('center_axis',(0.,0.,1.)) ;
#11657 = DIRECTION('ref_axis',(-1.,1.06581410364015E-13,0.)) ;
#11658 = DIRECTION('center_axis',(-0.381576765574097,0.921207802535445,-0.075995766473055)) ;
#11659 = DIRECTION('ref_axis',(0.924337152760837,0.380284934629309,-0.0313719065402705)) ;
#11660 = DIRECTION('center_axis',(-0.381576765574097,0.921207802535445,-0.075995766473055)) ;
#11661 = DIRECTION('ref_axis',(0.924337152760837,0.380284934629309,-0.0313719065402705)) ;
#11662 = DIRECTION('center_axis',(-0.381576765574099,-0.921207802535444,0.0759957664730568)) ;
#11663 = DIRECTION('ref_axis',(0.924337152760836,-0.380284934629311,0.0313719065402715)) ;
#11664 = DIRECTION('center_axis',(-0.381576765574099,-0.921207802535444,0.0759957664730568)) ;
#11665 = DIRECTION('ref_axis',(0.924337152760836,-0.380284934629311,0.0313719065402715)) ;
#11666 = DIRECTION('center_axis',(0.,0.,1.)) ;
#11667 = DIRECTION('ref_axis',(-0.707106781186494,0.707106781186601,0.)) ;
#11668 = DIRECTION('center_axis',(0.381576765574099,0.921207802535444,-0.0759957664730568)) ;
#11669 = DIRECTION('ref_axis',(0.924337152760836,-0.380284934629311,0.0313719065402715)) ;
#11670 = DIRECTION('center_axis',(0.381576765574099,0.921207802535444,-0.0759957664730568)) ;
#11671 = DIRECTION('ref_axis',(0.924337152760836,-0.380284934629311,0.0313719065402715)) ;
#11672 = DIRECTION('center_axis',(-0.921207802535445,-0.381576765574097,0.0759957664730571)) ;
#11673 = DIRECTION('ref_axis',(0.389070924829673,-0.903463793566638,0.17993606966465)) ;
#11674 = DIRECTION('center_axis',(-0.921207802535445,-0.381576765574097,0.0759957664730571)) ;
#11675 = DIRECTION('ref_axis',(0.389070924829673,-0.903463793566638,0.17993606966465)) ;
#11676 = DIRECTION('center_axis',(0.,0.,1.)) ;
#11677 = DIRECTION('ref_axis',(1.,0.,0.)) ;
#11678 = DIRECTION('center_axis',(0.921207802535445,0.381576765574097,-0.0759957664730571)) ;
#11679 = DIRECTION('ref_axis',(0.389070924829673,-0.903463793566638,0.17993606966465)) ;
#11680 = DIRECTION('center_axis',(0.921207802535445,0.381576765574097,-0.0759957664730571)) ;
#11681 = DIRECTION('ref_axis',(0.389070924829673,-0.903463793566638,0.17993606966465)) ;
#11682 = DIRECTION('center_axis',(-0.921207802535444,0.381576765574099,0.075995766473057)) ;
#11683 = DIRECTION('ref_axis',(0.389070924829674,0.903463793566638,0.179936069664649)) ;
#11684 = DIRECTION('center_axis',(0.,0.,1.)) ;
#11685 = DIRECTION('ref_axis',(1.,0.,0.)) ;
#11686 = DIRECTION('center_axis',(0.921207802535444,-0.381576765574099,-0.075995766473057)) ;
#11687 = DIRECTION('ref_axis',(0.389070924829674,0.903463793566638,0.179936069664649)) ;
#11688 = DIRECTION('center_axis',(-0.381576765574098,0.921207802535444,0.075995766473057)) ;
#11689 = DIRECTION('ref_axis',(0.924337152760836,0.380284934629311,0.0313719065402715)) ;
#11690 = DIRECTION('center_axis',(0.,0.,1.)) ;
#11691 = DIRECTION('ref_axis',(1.,0.,0.)) ;
#11692 = DIRECTION('center_axis',(0.381576765574098,-0.921207802535444,-0.075995766473057)) ;
#11693 = DIRECTION('ref_axis',(0.924337152760836,0.380284934629311,0.0313719065402715)) ;
#11694 = DIRECTION('center_axis',(0.381576765574099,0.921207802535444,0.075995766473055)) ;
#11695 = DIRECTION('ref_axis',(0.924337152760836,-0.380284934629311,-0.0313719065402707)) ;
#11696 = DIRECTION('center_axis',(0.,0.,1.)) ;
#11697 = DIRECTION('ref_axis',(1.,0.,0.)) ;
#11698 = DIRECTION('center_axis',(-0.381576765574099,-0.921207802535444,-0.075995766473055)) ;
#11699 = DIRECTION('ref_axis',(0.924337152760836,-0.380284934629311,-0.0313719065402707)) ;
#11700 = DIRECTION('center_axis',(0.921207802535444,0.381576765574099,0.075995766473057)) ;
#11701 = DIRECTION('ref_axis',(0.389070924829674,-0.903463793566638,-0.179936069664649)) ;
#11702 = DIRECTION('center_axis',(0.,0.,1.)) ;
#11703 = DIRECTION('ref_axis',(1.,0.,0.)) ;
#11704 = DIRECTION('center_axis',(-0.921207802535444,-0.381576765574099,-0.075995766473057)) ;
#11705 = DIRECTION('ref_axis',(0.389070924829674,-0.903463793566638,-0.179936069664649)) ;
#11706 = DIRECTION('center_axis',(0.921207802535445,-0.381576765574097,0.0759957664730568)) ;
#11707 = DIRECTION('ref_axis',(0.389070924829673,0.903463793566639,-0.179936069664649)) ;
#11708 = DIRECTION('center_axis',(0.921207802535445,-0.381576765574097,0.0759957664730568)) ;
#11709 = DIRECTION('ref_axis',(0.389070924829673,0.903463793566639,-0.179936069664649)) ;
#11710 = DIRECTION('center_axis',(0.,0.,1.)) ;
#11711 = DIRECTION('ref_axis',(-0.707106781186632,-0.707106781186463,0.)) ;
#11712 = DIRECTION('center_axis',(-0.921207802535445,0.381576765574097,-0.0759957664730568)) ;
#11713 = DIRECTION('ref_axis',(0.389070924829673,0.903463793566639,-0.179936069664649)) ;
#11714 = DIRECTION('center_axis',(-0.921207802535445,0.381576765574097,-0.0759957664730568)) ;
#11715 = DIRECTION('ref_axis',(0.389070924829673,0.903463793566639,-0.179936069664649)) ;
#11716 = DIRECTION('center_axis',(0.381576765574097,-0.921207802535445,0.075995766473057)) ;
#11717 = DIRECTION('ref_axis',(0.924337152760837,0.380284934629309,-0.0313719065402713)) ;
#11718 = DIRECTION('center_axis',(0.381576765574097,-0.921207802535445,0.075995766473057)) ;
#11719 = DIRECTION('ref_axis',(0.924337152760837,0.380284934629309,-0.0313719065402713)) ;
#11720 = DIRECTION('center_axis',(0.,0.,1.)) ;
#11721 = DIRECTION('ref_axis',(-1.,0.,0.)) ;
#11722 = DIRECTION('center_axis',(-0.381576765574097,0.921207802535445,-0.075995766473057)) ;
#11723 = DIRECTION('ref_axis',(0.924337152760837,0.380284934629309,-0.0313719065402713)) ;
#11724 = DIRECTION('center_axis',(-0.381576765574097,0.921207802535445,-0.075995766473057)) ;
#11725 = DIRECTION('ref_axis',(0.924337152760837,0.380284934629309,-0.0313719065402713)) ;
#11726 = DIRECTION('center_axis',(-0.381576765574097,-0.921207802535445,0.075995766473057)) ;
#11727 = DIRECTION('ref_axis',(0.924337152760837,-0.380284934629309,0.0313719065402713)) ;
#11728 = DIRECTION('center_axis',(-0.381576765574097,-0.921207802535445,0.075995766473057)) ;
#11729 = DIRECTION('ref_axis',(0.924337152760837,-0.380284934629309,0.0313719065402713)) ;
#11730 = DIRECTION('center_axis',(0.,0.,1.)) ;
#11731 = DIRECTION('ref_axis',(-0.707106781186601,0.707106781186494,0.)) ;
#11732 = DIRECTION('center_axis',(0.381576765574097,0.921207802535445,-0.075995766473057)) ;
#11733 = DIRECTION('ref_axis',(0.924337152760837,-0.380284934629309,0.0313719065402713)) ;
#11734 = DIRECTION('center_axis',(0.381576765574097,0.921207802535445,-0.075995766473057)) ;
#11735 = DIRECTION('ref_axis',(0.924337152760837,-0.380284934629309,0.0313719065402713)) ;
#11736 = DIRECTION('center_axis',(-0.921207802535445,-0.381576765574098,0.0759957664730548)) ;
#11737 = DIRECTION('ref_axis',(0.389070924829673,-0.90346379356664,0.179936069664645)) ;
#11738 = DIRECTION('center_axis',(-0.921207802535445,-0.381576765574098,0.0759957664730548)) ;
#11739 = DIRECTION('ref_axis',(0.389070924829673,-0.90346379356664,0.179936069664645)) ;
#11740 = DIRECTION('center_axis',(0.,0.,1.)) ;
#11741 = DIRECTION('ref_axis',(1.,0.,0.)) ;
#11742 = DIRECTION('center_axis',(0.921207802535445,0.381576765574098,-0.0759957664730548)) ;
#11743 = DIRECTION('ref_axis',(0.389070924829673,-0.90346379356664,0.179936069664645)) ;
#11744 = DIRECTION('center_axis',(0.921207802535445,0.381576765574098,-0.0759957664730548)) ;
#11745 = DIRECTION('ref_axis',(0.389070924829673,-0.90346379356664,0.179936069664645)) ;
#11746 = DIRECTION('center_axis',(-0.921207802535444,0.381576765574099,0.075995766473057)) ;
#11747 = DIRECTION('ref_axis',(0.389070924829674,0.903463793566638,0.179936069664649)) ;
#11748 = DIRECTION('center_axis',(0.,0.,1.)) ;
#11749 = DIRECTION('ref_axis',(1.,0.,0.)) ;
#11750 = DIRECTION('center_axis',(0.921207802535444,-0.381576765574099,-0.075995766473057)) ;
#11751 = DIRECTION('ref_axis',(0.389070924829674,0.903463793566638,0.179936069664649)) ;
#11752 = DIRECTION('center_axis',(-0.381576765574098,0.921207802535444,0.075995766473057)) ;
#11753 = DIRECTION('ref_axis',(0.924337152760836,0.380284934629311,0.0313719065402715)) ;
#11754 = DIRECTION('center_axis',(0.381576765574098,0.921207802535445,0.0759957664730569)) ;
#11755 = DIRECTION('ref_axis',(0.924337152760836,-0.38028493462931,-0.0313719065402714)) ;
#11756 = DIRECTION('center_axis',(0.381576765574098,0.921207802535445,0.0759957664730569)) ;
#11757 = DIRECTION('ref_axis',(0.924337152760836,-0.38028493462931,-0.0313719065402714)) ;
#11758 = DIRECTION('',(-0.381576765574098,-0.921207802535444,-0.0759957664730569)) ;
#11759 = DIRECTION('center_axis',(-0.704712865980969,-0.704712865980954,-0.0822165010311149)) ;
#11760 = DIRECTION('ref_axis',(0.70710678118654,-0.707106781186555,5.23532745586745E-15)) ;
#11761 = DIRECTION('center_axis',(-0.704712865980969,-0.704712865980954,-0.0822165010311149)) ;
#11762 = DIRECTION('ref_axis',(0.70710678118654,-0.707106781186555,5.23532745586745E-15)) ;
#11763 = DIRECTION('center_axis',(-0.704712865980969,-0.704712865980954,-0.0822165010311149)) ;
#11764 = DIRECTION('ref_axis',(0.70710678118654,-0.707106781186555,5.23532745586745E-15)) ;
#11765 = DIRECTION('center_axis',(0.381576765574098,0.921207802535445,0.0759957664730569)) ;
#11766 = DIRECTION('ref_axis',(0.924337152760836,-0.38028493462931,-0.0313719065402714)) ;
#11767 = DIRECTION('center_axis',(0.921207802535446,0.381576765574096,0.0759957664730549)) ;
#11768 = DIRECTION('ref_axis',(0.389070924829671,-0.90346379356664,-0.179936069664646)) ;
#11769 = DIRECTION('',(-0.921207802535446,-0.381576765574096,-0.0759957664730549)) ;
#11770 = DIRECTION('center_axis',(-0.996614492649089,-1.90638497962248E-14,
-0.0822165010311158)) ;
#11771 = DIRECTION('ref_axis',(1.78786833485215E-14,-1.,1.54574446170177E-14)) ;
#11772 = DIRECTION('center_axis',(-0.996614492649089,-1.90638497962248E-14,
-0.0822165010311158)) ;
#11773 = DIRECTION('ref_axis',(1.78786833485215E-14,-1.,1.54574446170177E-14)) ;
#11774 = DIRECTION('center_axis',(0.921207802535444,-0.381576765574099,0.075995766473057)) ;
#11775 = DIRECTION('ref_axis',(0.389070924829674,0.903463793566638,-0.179936069664649)) ;
#11776 = DIRECTION('',(-0.921207802535444,0.381576765574099,-0.075995766473057)) ;
#11777 = DIRECTION('center_axis',(-0.704712865980983,0.70471286598094,-0.0822165010311149)) ;
#11778 = DIRECTION('ref_axis',(0.707106781186526,0.707106781186569,-7.7287223085089E-15)) ;
#11779 = DIRECTION('center_axis',(0.381576765574096,-0.921207802535445,0.0759957664730569)) ;
#11780 = DIRECTION('ref_axis',(0.924337152760837,0.380284934629308,-0.0313719065402712)) ;
#11781 = DIRECTION('',(-0.381576765574096,0.921207802535445,-0.0759957664730569)) ;
#11782 = DIRECTION('center_axis',(8.18196890271355E-15,0.996614492649089,
-0.0822165010311158)) ;
#11783 = DIRECTION('ref_axis',(1.,-8.08148556740336E-15,6.73457130616947E-16)) ;
#11784 = DIRECTION('center_axis',(-0.3815767655741,-0.921207802535444,0.0759957664730569)) ;
#11785 = DIRECTION('ref_axis',(0.924337152760836,-0.380284934629312,0.0313719065402716)) ;
#11786 = DIRECTION('',(0.3815767655741,0.921207802535444,-0.0759957664730569)) ;
#11787 = DIRECTION('center_axis',(0.704712865980961,0.704712865980961,-0.0822165010311149)) ;
#11788 = DIRECTION('ref_axis',(0.707106781186547,-0.707106781186548,-5.99697540120808E-15)) ;
#11789 = DIRECTION('center_axis',(-0.921207802535445,-0.381576765574097,0.0759957664730571)) ;
#11790 = DIRECTION('ref_axis',(0.389070924829673,-0.903463793566638,0.17993606966465)) ;
#11791 = DIRECTION('',(0.921207802535445,0.381576765574097,-0.0759957664730571)) ;
#11792 = DIRECTION('center_axis',(0.996614492649089,1.34995599539884E-15,
-0.0822165010311158)) ;
#11793 = DIRECTION('ref_axis',(7.0352218109092E-16,-1.,-7.98527740588669E-15)) ;
#11794 = DIRECTION('center_axis',(0.996614492649089,1.34995599539884E-15,
-0.0822165010311158)) ;
#11795 = DIRECTION('ref_axis',(7.0352218109092E-16,-1.,-7.98527740588669E-15)) ;
#11796 = DIRECTION('center_axis',(-0.921207802535444,0.381576765574099,0.075995766473057)) ;
#11797 = DIRECTION('ref_axis',(0.389070924829674,0.903463793566638,0.179936069664649)) ;
#11798 = DIRECTION('',(0.921207802535444,-0.381576765574099,-0.075995766473057)) ;
#11799 = DIRECTION('center_axis',(0.704712865980961,-0.704712865980961,-0.0822165010311149)) ;
#11800 = DIRECTION('ref_axis',(0.707106781186548,0.707106781186547,5.35558765776336E-15)) ;
#11801 = DIRECTION('center_axis',(0.704712865980961,-0.704712865980961,-0.0822165010311149)) ;
#11802 = DIRECTION('ref_axis',(0.707106781186548,0.707106781186547,5.35558765776336E-15)) ;
#11803 = DIRECTION('center_axis',(0.704712865980961,-0.704712865980961,-0.0822165010311149)) ;
#11804 = DIRECTION('ref_axis',(0.707106781186548,0.707106781186547,5.35558765776336E-15)) ;
#11805 = DIRECTION('center_axis',(-0.381576765574098,0.921207802535444,0.075995766473057)) ;
#11806 = DIRECTION('ref_axis',(0.924337152760836,0.380284934629311,0.0313719065402715)) ;
#11807 = DIRECTION('',(0.381576765574098,-0.921207802535444,-0.075995766473057)) ;
#11808 = DIRECTION('center_axis',(0.,-0.996614492649089,-0.0822165010311158)) ;
#11809 = DIRECTION('ref_axis',(1.,0.,4.00867339652946E-18)) ;
#11810 = DIRECTION('center_axis',(0.,-0.996614492649089,-0.0822165010311158)) ;
#11811 = DIRECTION('ref_axis',(1.,0.,4.00867339652946E-18)) ;
#11812 = DIRECTION('center_axis',(0.381576765574098,0.921207802535445,0.0759957664730568)) ;
#11813 = DIRECTION('ref_axis',(0.924337152760837,-0.38028493462931,-0.0313719065402713)) ;
#11814 = DIRECTION('',(-0.381576765574098,-0.921207802535445,-0.0759957664730568)) ;
#11815 = DIRECTION('center_axis',(-0.704712865980969,-0.704712865980953,-0.0822165010311149)) ;
#11816 = DIRECTION('ref_axis',(0.707106781186539,-0.707106781186556,5.30748357700498E-15)) ;
#11817 = DIRECTION('center_axis',(-0.704712865980969,-0.704712865980953,-0.0822165010311149)) ;
#11818 = DIRECTION('ref_axis',(0.707106781186539,-0.707106781186556,5.30748357700498E-15)) ;
#11819 = DIRECTION('center_axis',(-0.704712865980969,-0.704712865980953,-0.0822165010311149)) ;
#11820 = DIRECTION('ref_axis',(0.707106781186539,-0.707106781186556,5.30748357700498E-15)) ;
#11821 = DIRECTION('center_axis',(0.921207802535445,0.381576765574097,0.0759957664730571)) ;
#11822 = DIRECTION('ref_axis',(0.389070924829673,-0.903463793566638,-0.17993606966465)) ;
#11823 = DIRECTION('',(-0.921207802535445,-0.381576765574097,-0.0759957664730571)) ;
#11824 = DIRECTION('center_axis',(-0.996614492649089,-1.34995599539884E-15,
-0.0822165010311158)) ;
#11825 = DIRECTION('ref_axis',(7.0352218109092E-16,-1.,7.98527740588669E-15)) ;
#11826 = DIRECTION('center_axis',(-0.996614492649089,-1.34995599539884E-15,
-0.0822165010311158)) ;
#11827 = DIRECTION('ref_axis',(7.0352218109092E-16,-1.,7.98527740588669E-15)) ;
#11828 = DIRECTION('center_axis',(0.921207802535445,-0.381576765574097,0.0759957664730568)) ;
#11829 = DIRECTION('ref_axis',(0.389070924829672,0.903463793566639,-0.179936069664649)) ;
#11830 = DIRECTION('',(-0.921207802535445,0.381576765574097,-0.0759957664730568)) ;
#11831 = DIRECTION('center_axis',(-0.70471286598097,0.704712865980952,-0.0822165010311149)) ;
#11832 = DIRECTION('ref_axis',(0.707106781186539,0.707106781186556,-6.87888354844459E-15)) ;
#11833 = DIRECTION('center_axis',(0.381576765574097,-0.921207802535445,0.075995766473055)) ;
#11834 = DIRECTION('ref_axis',(0.924337152760837,0.380284934629309,-0.0313719065402705)) ;
#11835 = DIRECTION('',(-0.381576765574097,0.921207802535445,-0.075995766473055)) ;
#11836 = DIRECTION('center_axis',(8.18196890271356E-15,0.99661449264909,-0.082216501031107)) ;
#11837 = DIRECTION('ref_axis',(1.,-8.14562434174784E-15,6.73457130616947E-16)) ;
#11838 = DIRECTION('center_axis',(-0.381576765574099,-0.921207802535444,0.0759957664730568)) ;
#11839 = DIRECTION('ref_axis',(0.924337152760836,-0.380284934629311,0.0313719065402715)) ;
#11840 = DIRECTION('',(0.381576765574099,0.921207802535444,-0.0759957664730568)) ;
#11841 = DIRECTION('center_axis',(0.704712865980969,0.704712865980953,-0.0822165010311149)) ;
#11842 = DIRECTION('ref_axis',(0.707106781186539,-0.707106781186556,-5.58007336796898E-15)) ;
#11843 = DIRECTION('center_axis',(-0.921207802535445,-0.381576765574097,0.0759957664730571)) ;
#11844 = DIRECTION('ref_axis',(0.389070924829673,-0.903463793566638,0.17993606966465)) ;
#11845 = DIRECTION('',(0.921207802535445,0.381576765574097,-0.0759957664730571)) ;
#11846 = DIRECTION('center_axis',(0.996614492649089,1.34995599539884E-15,
-0.0822165010311158)) ;
#11847 = DIRECTION('ref_axis',(7.0352218109092E-16,-1.,-7.98527740588669E-15)) ;
#11848 = DIRECTION('center_axis',(0.996614492649089,1.34995599539884E-15,
-0.0822165010311158)) ;
#11849 = DIRECTION('ref_axis',(7.0352218109092E-16,-1.,-7.98527740588669E-15)) ;
#11850 = DIRECTION('center_axis',(-0.921207802535444,0.381576765574099,0.075995766473057)) ;
#11851 = DIRECTION('ref_axis',(0.389070924829674,0.903463793566638,0.179936069664649)) ;
#11852 = DIRECTION('',(0.921207802535444,-0.381576765574099,-0.075995766473057)) ;
#11853 = DIRECTION('center_axis',(0.704712865980961,-0.704712865980961,-0.0822165010311149)) ;
#11854 = DIRECTION('ref_axis',(0.707106781186548,0.707106781186547,5.35558765776336E-15)) ;
#11855 = DIRECTION('center_axis',(0.704712865980961,-0.704712865980961,-0.0822165010311149)) ;
#11856 = DIRECTION('ref_axis',(0.707106781186548,0.707106781186547,5.35558765776336E-15)) ;
#11857 = DIRECTION('center_axis',(0.704712865980961,-0.704712865980961,-0.0822165010311149)) ;
#11858 = DIRECTION('ref_axis',(0.707106781186548,0.707106781186547,5.35558765776336E-15)) ;
#11859 = DIRECTION('center_axis',(-0.381576765574098,0.921207802535444,0.075995766473057)) ;
#11860 = DIRECTION('ref_axis',(0.924337152760836,0.380284934629311,0.0313719065402715)) ;
#11861 = DIRECTION('',(0.381576765574098,-0.921207802535444,-0.075995766473057)) ;
#11862 = DIRECTION('center_axis',(-6.83201290731471E-15,-0.996614492649089,
-0.0822165010311158)) ;
#11863 = DIRECTION('ref_axis',(1.,-6.79871008051394E-15,-5.57205602117593E-16)) ;
#11864 = DIRECTION('center_axis',(-6.83201290731471E-15,-0.996614492649089,
-0.0822165010311158)) ;
#11865 = DIRECTION('ref_axis',(1.,-6.79871008051394E-15,-5.57205602117593E-16)) ;
#11866 = DIRECTION('center_axis',(0.381576765574099,0.921207802535444,0.075995766473055)) ;
#11867 = DIRECTION('ref_axis',(0.924337152760836,-0.380284934629311,-0.0313719065402707)) ;
#11868 = DIRECTION('',(-0.381576765574099,-0.921207802535444,-0.075995766473055)) ;
#11869 = DIRECTION('center_axis',(-0.704712865980962,-0.70471286598096,-0.0822165010311149)) ;
#11870 = DIRECTION('ref_axis',(0.707106781186546,-0.707106781186549,1.06630712347684E-14)) ;
#11871 = DIRECTION('center_axis',(-0.704712865980962,-0.70471286598096,-0.0822165010311149)) ;
#11872 = DIRECTION('ref_axis',(0.707106781186546,-0.707106781186549,1.06630712347684E-14)) ;
#11873 = DIRECTION('center_axis',(-0.704712865980962,-0.70471286598096,-0.0822165010311149)) ;
#11874 = DIRECTION('ref_axis',(0.707106781186546,-0.707106781186549,1.06630712347684E-14)) ;
#11875 = DIRECTION('center_axis',(0.921207802535444,0.381576765574099,0.075995766473057)) ;
#11876 = DIRECTION('ref_axis',(0.389070924829674,-0.903463793566638,-0.179936069664649)) ;
#11877 = DIRECTION('',(-0.921207802535444,-0.381576765574099,-0.075995766473057)) ;
#11878 = DIRECTION('center_axis',(-0.996614492649089,-1.34995599539884E-15,
-0.0822165010311158)) ;
#11879 = DIRECTION('ref_axis',(7.3759590496142E-16,-1.,8.33804066478127E-15)) ;
#11880 = DIRECTION('center_axis',(-0.996614492649089,-1.34995599539884E-15,
-0.0822165010311158)) ;
#11881 = DIRECTION('ref_axis',(7.3759590496142E-16,-1.,8.33804066478127E-15)) ;
#11882 = DIRECTION('center_axis',(0.921207802535445,-0.381576765574097,0.0759957664730568)) ;
#11883 = DIRECTION('ref_axis',(0.389070924829673,0.903463793566639,-0.179936069664649)) ;
#11884 = DIRECTION('',(-0.921207802535445,0.381576765574097,-0.0759957664730568)) ;
#11885 = DIRECTION('center_axis',(-0.704712865980969,0.704712865980953,-0.0822165010311149)) ;
#11886 = DIRECTION('ref_axis',(0.70710678118654,0.707106781186555,-6.95905701637518E-15)) ;
#11887 = DIRECTION('center_axis',(0.381576765574097,-0.921207802535445,0.075995766473057)) ;
#11888 = DIRECTION('ref_axis',(0.924337152760837,0.380284934629309,-0.0313719065402713)) ;
#11889 = DIRECTION('',(-0.381576765574097,0.921207802535445,-0.075995766473057)) ;
#11890 = DIRECTION('center_axis',(0.,0.996614492649089,-0.0822165010311159)) ;
#11891 = DIRECTION('ref_axis',(1.,0.,-4.00867339652946E-18)) ;
#11892 = DIRECTION('center_axis',(-0.381576765574097,-0.921207802535445,0.075995766473057)) ;
#11893 = DIRECTION('ref_axis',(0.924337152760837,-0.380284934629309,0.0313719065402713)) ;
#11894 = DIRECTION('',(0.381576765574097,0.921207802535445,-0.075995766473057)) ;
#11895 = DIRECTION('center_axis',(0.704712865980961,0.704712865980961,-0.0822165010311149)) ;
#11896 = DIRECTION('ref_axis',(0.707106781186547,-0.707106781186548,-5.54800398079677E-15)) ;
#11897 = DIRECTION('center_axis',(-0.921207802535445,-0.381576765574098,0.0759957664730548)) ;
#11898 = DIRECTION('ref_axis',(0.389070924829673,-0.90346379356664,0.179936069664645)) ;
#11899 = DIRECTION('',(0.921207802535445,0.381576765574098,-0.0759957664730548)) ;
#11900 = DIRECTION('center_axis',(0.996614492649089,1.34995599539885E-15,
-0.0822165010311166)) ;
#11901 = DIRECTION('ref_axis',(1.46316578973325E-16,-1.,-1.54895140041898E-14)) ;
#11902 = DIRECTION('center_axis',(0.996614492649089,1.34995599539885E-15,
-0.0822165010311166)) ;
#11903 = DIRECTION('ref_axis',(1.46316578973325E-16,-1.,-1.54895140041898E-14)) ;
#11904 = DIRECTION('center_axis',(-0.921207802535444,0.381576765574099,0.075995766473057)) ;
#11905 = DIRECTION('ref_axis',(0.389070924829674,0.903463793566638,0.179936069664649)) ;
#11906 = DIRECTION('',(0.921207802535444,-0.381576765574099,-0.075995766473057)) ;
#11907 = DIRECTION('center_axis',(0.704712865980961,-0.704712865980961,-0.0822165010311149)) ;
#11908 = DIRECTION('ref_axis',(0.707106781186548,0.707106781186547,5.35558765776336E-15)) ;
#11909 = DIRECTION('center_axis',(0.704712865980961,-0.704712865980961,-0.0822165010311149)) ;
#11910 = DIRECTION('ref_axis',(0.707106781186548,0.707106781186547,5.35558765776336E-15)) ;
#11911 = DIRECTION('center_axis',(0.704712865980961,-0.704712865980961,-0.0822165010311149)) ;
#11912 = DIRECTION('ref_axis',(0.707106781186548,0.707106781186547,5.35558765776336E-15)) ;
#11913 = DIRECTION('center_axis',(-0.381576765574098,0.921207802535444,0.075995766473057)) ;
#11914 = DIRECTION('ref_axis',(0.924337152760836,0.380284934629311,0.0313719065402715)) ;
#11915 = DIRECTION('',(0.381576765574098,-0.921207802535444,-0.075995766473057)) ;
#11916 = DIRECTION('center_axis',(0.381576765574098,-0.921207802535444,-0.075995766473057)) ;
#11917 = DIRECTION('ref_axis',(0.924337152760836,0.380284934629311,0.0313719065402715)) ;
#11918 = DIRECTION('center_axis',(0.381576765574098,-0.921207802535444,-0.075995766473057)) ;
#11919 = DIRECTION('ref_axis',(-0.924337152760836,-0.380284934629311,-0.0313719065402715)) ;
#11920 = DIRECTION('axis',(0.,0.,1.)) ;
#11921 = DIRECTION('refdir',(1.,0.,0.)) ;
#11922 = DIRECTION('center_axis',(0.,0.,1.)) ;
#11923 = DIRECTION('ref_axis',(1.,0.,0.)) ;
#11924 = DIRECTION('center_axis',(0.,0.,1.)) ;
#11925 = DIRECTION('ref_axis',(1.,0.,0.)) ;
#11926 = DIRECTION('',(0.,0.,-1.)) ;
#11927 = DIRECTION('center_axis',(0.,0.,-1.)) ;
#11928 = DIRECTION('ref_axis',(1.,0.,0.)) ;
#11929 = DIRECTION('center_axis',(0.,0.,1.)) ;
#11930 = DIRECTION('ref_axis',(1.,0.,0.)) ;
#11931 = DIRECTION('center_axis',(0.,0.,1.)) ;
#11932 = DIRECTION('ref_axis',(1.,0.,0.)) ;
#11933 = DIRECTION('',(0.,1.,0.)) ;
#11934 = DIRECTION('',(-1.,0.,0.)) ;
#11935 = DIRECTION('',(0.,-1.,0.)) ;
#11936 = DIRECTION('',(1.,0.,0.)) ;
#11937 = DIRECTION('center_axis',(0.,0.,1.)) ;
#11938 = DIRECTION('ref_axis',(1.,0.,0.)) ;
#11939 = DIRECTION('',(0.,-1.,0.)) ;
#11940 = DIRECTION('',(-1.,0.,0.)) ;
#11941 = DIRECTION('',(0.,1.,0.)) ;
#11942 = DIRECTION('',(1.,0.,0.)) ;
#11943 = DIRECTION('center_axis',(0.,1.,0.)) ;
#11944 = DIRECTION('ref_axis',(0.,0.,1.)) ;
#11945 = DIRECTION('',(0.,0.,-1.)) ;
#11946 = DIRECTION('',(0.,0.,-1.)) ;
#11947 = DIRECTION('center_axis',(1.,0.,0.)) ;
#11948 = DIRECTION('ref_axis',(0.,0.,-1.)) ;
#11949 = DIRECTION('',(0.,0.,-1.)) ;
#11950 = DIRECTION('center_axis',(0.,-1.,0.)) ;
#11951 = DIRECTION('ref_axis',(0.,0.,-1.)) ;
#11952 = DIRECTION('',(0.,0.,-1.)) ;
#11953 = DIRECTION('center_axis',(-1.,0.,0.)) ;
#11954 = DIRECTION('ref_axis',(0.,0.,1.)) ;
#11955 = DIRECTION('axis',(0.,0.,1.)) ;
#11956 = DIRECTION('refdir',(1.,0.,0.)) ;
#11957 = DIRECTION('center_axis',(0.,0.,1.)) ;
#11958 = DIRECTION('ref_axis',(1.,0.,0.)) ;
#11959 = DIRECTION('center_axis',(0.,0.,1.)) ;
#11960 = DIRECTION('ref_axis',(1.,0.,0.)) ;
#11961 = DIRECTION('',(0.,0.,-1.)) ;
#11962 = DIRECTION('center_axis',(0.,0.,-1.)) ;
#11963 = DIRECTION('ref_axis',(1.,0.,0.)) ;
#11964 = DIRECTION('center_axis',(0.,0.,-1.)) ;
#11965 = DIRECTION('ref_axis',(-1.,0.,0.)) ;
#11966 = DIRECTION('center_axis',(0.,0.,1.)) ;
#11967 = DIRECTION('ref_axis',(1.,0.,0.)) ;
#11968 = DIRECTION('center_axis',(0.,0.,1.)) ;
#11969 = DIRECTION('ref_axis',(1.,0.,0.)) ;
#11970 = DIRECTION('center_axis',(0.,0.,1.)) ;
#11971 = DIRECTION('ref_axis',(1.,0.,0.)) ;
#11972 = DIRECTION('',(0.,0.,-1.)) ;
#11973 = DIRECTION('center_axis',(0.,0.,-1.)) ;
#11974 = DIRECTION('ref_axis',(1.,0.,0.)) ;
#11975 = DIRECTION('center_axis',(0.,0.,-1.)) ;
#11976 = DIRECTION('ref_axis',(-1.,0.,0.)) ;
#11977 = DIRECTION('center_axis',(0.,0.,1.)) ;
#11978 = DIRECTION('ref_axis',(1.,0.,0.)) ;
#11979 = DIRECTION('axis',(0.,0.,1.)) ;
#11980 = DIRECTION('refdir',(1.,0.,0.)) ;
#11981 = DIRECTION('center_axis',(0.,0.,1.)) ;
#11982 = DIRECTION('ref_axis',(1.,0.,0.)) ;
#11983 = DIRECTION('center_axis',(0.,0.,1.)) ;
#11984 = DIRECTION('ref_axis',(1.,0.,0.)) ;
#11985 = DIRECTION('',(0.,0.,-1.)) ;
#11986 = DIRECTION('center_axis',(0.,0.,-1.)) ;
#11987 = DIRECTION('ref_axis',(1.,0.,0.)) ;
#11988 = DIRECTION('center_axis',(0.,0.,-1.)) ;
#11989 = DIRECTION('ref_axis',(-1.,0.,0.)) ;
#11990 = DIRECTION('center_axis',(0.,0.,1.)) ;
#11991 = DIRECTION('ref_axis',(1.,0.,0.)) ;
#11992 = DIRECTION('axis',(0.,0.,1.)) ;
#11993 = DIRECTION('refdir',(1.,0.,0.)) ;
#11994 = DIRECTION('center_axis',(0.,0.,1.)) ;
#11995 = DIRECTION('ref_axis',(1.,0.,0.)) ;
#11996 = DIRECTION('center_axis',(0.,0.,1.)) ;
#11997 = DIRECTION('ref_axis',(1.,0.,0.)) ;
#11998 = DIRECTION('',(0.,0.,-1.)) ;
#11999 = DIRECTION('center_axis',(0.,0.,-1.)) ;
#12000 = DIRECTION('ref_axis',(1.,0.,0.)) ;
#12001 = DIRECTION('center_axis',(0.,0.,-1.)) ;
#12002 = DIRECTION('ref_axis',(-1.,0.,0.)) ;
#12003 = DIRECTION('center_axis',(0.,0.,1.)) ;
#12004 = DIRECTION('ref_axis',(1.,0.,0.)) ;
#12005 = DIRECTION('axis',(0.,0.,1.)) ;
#12006 = DIRECTION('refdir',(1.,0.,0.)) ;
#12007 = DIRECTION('center_axis',(0.,0.,1.)) ;
#12008 = DIRECTION('ref_axis',(1.,0.,0.)) ;
#12009 = DIRECTION('center_axis',(-0.381869435050518,-0.921914369154711,-0.0651891902102614)) ;
#12010 = DIRECTION('ref_axis',(0.924216281275221,-0.38091832663704,-0.0269349931843283)) ;
#12011 = DIRECTION('center_axis',(0.921914369154713,0.381869435050514,0.0651891902102614)) ;
#12012 = DIRECTION('ref_axis',(0.38739372213043,-0.908767745068236,-0.155136358012961)) ;
#12013 = DIRECTION('center_axis',(0.,0.,1.)) ;
#12014 = DIRECTION('ref_axis',(1.,0.,0.)) ;
#12015 = DIRECTION('center_axis',(-0.921914369154713,-0.381869435050514,-0.0651891902102614)) ;
#12016 = DIRECTION('ref_axis',(0.38739372213043,-0.908767745068236,-0.155136358012961)) ;
#12017 = DIRECTION('center_axis',(0.921914369154711,-0.381869435050519,0.0651891902102617)) ;
#12018 = DIRECTION('ref_axis',(0.387393722130434,0.908767745068234,-0.155136358012959)) ;
#12019 = DIRECTION('center_axis',(0.921914369154711,-0.381869435050519,0.0651891902102617)) ;
#12020 = DIRECTION('ref_axis',(0.387393722130434,0.908767745068234,-0.155136358012959)) ;
#12021 = DIRECTION('center_axis',(0.,0.,1.)) ;
#12022 = DIRECTION('ref_axis',(-0.707106781186548,-0.707106781186548,0.)) ;
#12023 = DIRECTION('center_axis',(-0.921914369154711,0.381869435050519,-0.0651891902102617)) ;
#12024 = DIRECTION('ref_axis',(0.387393722130434,0.908767745068234,-0.155136358012959)) ;
#12025 = DIRECTION('center_axis',(-0.921914369154711,0.381869435050519,-0.0651891902102617)) ;
#12026 = DIRECTION('ref_axis',(0.387393722130434,0.908767745068234,-0.155136358012959)) ;
#12027 = DIRECTION('center_axis',(0.381869435050516,-0.921914369154712,0.0651891902102615)) ;
#12028 = DIRECTION('ref_axis',(0.924216281275222,0.380918326637037,-0.0269349931843281)) ;
#12029 = DIRECTION('center_axis',(0.381869435050516,-0.921914369154712,0.0651891902102615)) ;
#12030 = DIRECTION('ref_axis',(0.924216281275222,0.380918326637037,-0.0269349931843281)) ;
#12031 = DIRECTION('center_axis',(0.,0.,1.)) ;
#12032 = DIRECTION('ref_axis',(-1.,0.,0.)) ;
#12033 = DIRECTION('center_axis',(-0.381869435050516,0.921914369154712,-0.0651891902102615)) ;
#12034 = DIRECTION('ref_axis',(0.924216281275222,0.380918326637037,-0.0269349931843281)) ;
#12035 = DIRECTION('center_axis',(-0.381869435050516,0.921914369154712,-0.0651891902102615)) ;
#12036 = DIRECTION('ref_axis',(0.924216281275222,0.380918326637037,-0.0269349931843281)) ;
#12037 = DIRECTION('center_axis',(-0.381869435050518,-0.921914369154711,0.0651891902102613)) ;
#12038 = DIRECTION('ref_axis',(0.924216281275221,-0.380918326637039,0.0269349931843282)) ;
#12039 = DIRECTION('center_axis',(-0.381869435050518,-0.921914369154711,0.0651891902102613)) ;
#12040 = DIRECTION('ref_axis',(0.924216281275221,-0.380918326637039,0.0269349931843282)) ;
#12041 = DIRECTION('center_axis',(0.,0.,1.)) ;
#12042 = DIRECTION('ref_axis',(-0.707106781186509,0.707106781186586,0.)) ;
#12043 = DIRECTION('center_axis',(0.381869435050518,0.921914369154711,-0.0651891902102613)) ;
#12044 = DIRECTION('ref_axis',(0.924216281275221,-0.380918326637039,0.0269349931843282)) ;
#12045 = DIRECTION('center_axis',(0.381869435050518,0.921914369154711,-0.0651891902102613)) ;
#12046 = DIRECTION('ref_axis',(0.924216281275221,-0.380918326637039,0.0269349931843282)) ;
#12047 = DIRECTION('center_axis',(-0.921914369154711,-0.381869435050517,0.0651891902102618)) ;
#12048 = DIRECTION('ref_axis',(0.387393722130432,-0.908767745068235,0.15513635801296)) ;
#12049 = DIRECTION('center_axis',(-0.921914369154711,-0.381869435050517,0.0651891902102618)) ;
#12050 = DIRECTION('ref_axis',(0.387393722130432,-0.908767745068235,0.15513635801296)) ;
#12051 = DIRECTION('center_axis',(0.,0.,1.)) ;
#12052 = DIRECTION('ref_axis',(1.,0.,0.)) ;
#12053 = DIRECTION('center_axis',(0.921914369154711,0.381869435050517,-0.0651891902102618)) ;
#12054 = DIRECTION('ref_axis',(0.387393722130432,-0.908767745068235,0.15513635801296)) ;
#12055 = DIRECTION('center_axis',(0.921914369154711,0.381869435050517,-0.0651891902102618)) ;
#12056 = DIRECTION('ref_axis',(0.387393722130432,-0.908767745068235,0.15513635801296)) ;
#12057 = DIRECTION('center_axis',(-0.921914369154711,0.381869435050517,0.0651891902102614)) ;
#12058 = DIRECTION('ref_axis',(0.387393722130432,0.908767745068235,0.155136358012959)) ;
#12059 = DIRECTION('center_axis',(0.,0.,1.)) ;
#12060 = DIRECTION('ref_axis',(1.,0.,0.)) ;
#12061 = DIRECTION('center_axis',(0.921914369154711,-0.381869435050517,-0.0651891902102614)) ;
#12062 = DIRECTION('ref_axis',(0.387393722130432,0.908767745068235,0.155136358012959)) ;
#12063 = DIRECTION('center_axis',(-0.381869435050518,0.921914369154711,0.0651891902102615)) ;
#12064 = DIRECTION('ref_axis',(0.924216281275221,0.380918326637039,0.0269349931843283)) ;
#12065 = DIRECTION('center_axis',(0.,0.,1.)) ;
#12066 = DIRECTION('ref_axis',(1.,0.,0.)) ;
#12067 = DIRECTION('center_axis',(0.381869435050518,-0.921914369154711,-0.0651891902102615)) ;
#12068 = DIRECTION('ref_axis',(0.924216281275221,0.380918326637039,0.0269349931843283)) ;
#12069 = DIRECTION('center_axis',(0.381869435050518,0.921914369154711,0.0651891902102614)) ;
#12070 = DIRECTION('ref_axis',(0.924216281275221,-0.38091832663704,-0.0269349931843283)) ;
#12071 = DIRECTION('center_axis',(0.,0.,1.)) ;
#12072 = DIRECTION('ref_axis',(1.,0.,0.)) ;
#12073 = DIRECTION('center_axis',(-0.381869435050518,-0.921914369154711,-0.0651891902102614)) ;
#12074 = DIRECTION('ref_axis',(0.924216281275221,-0.38091832663704,-0.0269349931843283)) ;
#12075 = DIRECTION('center_axis',(0.921914369154711,0.381869435050517,0.0651891902102614)) ;
#12076 = DIRECTION('ref_axis',(0.387393722130433,-0.908767745068235,-0.155136358012959)) ;
#12077 = DIRECTION('center_axis',(0.,0.,1.)) ;
#12078 = DIRECTION('ref_axis',(1.,0.,0.)) ;
#12079 = DIRECTION('center_axis',(-0.921914369154711,-0.381869435050517,-0.0651891902102614)) ;
#12080 = DIRECTION('ref_axis',(0.387393722130433,-0.908767745068235,-0.155136358012959)) ;
#12081 = DIRECTION('center_axis',(0.921914369154711,-0.381869435050518,0.0651891902102616)) ;
#12082 = DIRECTION('ref_axis',(0.387393722130434,0.908767745068234,-0.155136358012959)) ;
#12083 = DIRECTION('center_axis',(0.921914369154711,-0.381869435050518,0.0651891902102616)) ;
#12084 = DIRECTION('ref_axis',(0.387393722130434,0.908767745068234,-0.155136358012959)) ;
#12085 = DIRECTION('center_axis',(0.,0.,1.)) ;
#12086 = DIRECTION('ref_axis',(-0.707106781186703,-0.707106781186392,0.)) ;
#12087 = DIRECTION('center_axis',(-0.921914369154711,0.381869435050518,-0.0651891902102616)) ;
#12088 = DIRECTION('ref_axis',(0.387393722130434,0.908767745068234,-0.155136358012959)) ;
#12089 = DIRECTION('center_axis',(-0.921914369154711,0.381869435050518,-0.0651891902102616)) ;
#12090 = DIRECTION('ref_axis',(0.387393722130434,0.908767745068234,-0.155136358012959)) ;
#12091 = DIRECTION('center_axis',(0.381869435050516,-0.921914369154712,0.0651891902102615)) ;
#12092 = DIRECTION('ref_axis',(0.924216281275222,0.380918326637037,-0.0269349931843281)) ;
#12093 = DIRECTION('center_axis',(0.381869435050516,-0.921914369154712,0.0651891902102615)) ;
#12094 = DIRECTION('ref_axis',(0.924216281275222,0.380918326637037,-0.0269349931843281)) ;
#12095 = DIRECTION('center_axis',(0.,0.,1.)) ;
#12096 = DIRECTION('ref_axis',(-1.,1.55431223447522E-13,0.)) ;
#12097 = DIRECTION('center_axis',(-0.381869435050516,0.921914369154712,-0.0651891902102615)) ;
#12098 = DIRECTION('ref_axis',(0.924216281275222,0.380918326637037,-0.0269349931843281)) ;
#12099 = DIRECTION('center_axis',(-0.381869435050516,0.921914369154712,-0.0651891902102615)) ;
#12100 = DIRECTION('ref_axis',(0.924216281275222,0.380918326637037,-0.0269349931843281)) ;
#12101 = DIRECTION('center_axis',(-0.381869435050519,-0.921914369154711,0.0651891902102615)) ;
#12102 = DIRECTION('ref_axis',(0.92421628127522,-0.38091832663704,0.0269349931843284)) ;
#12103 = DIRECTION('center_axis',(-0.381869435050519,-0.921914369154711,0.0651891902102615)) ;
#12104 = DIRECTION('ref_axis',(0.92421628127522,-0.38091832663704,0.0269349931843284)) ;
#12105 = DIRECTION('center_axis',(0.,0.,1.)) ;
#12106 = DIRECTION('ref_axis',(-0.707106781186548,0.707106781186548,0.)) ;
#12107 = DIRECTION('center_axis',(0.381869435050519,0.921914369154711,-0.0651891902102615)) ;
#12108 = DIRECTION('ref_axis',(0.92421628127522,-0.38091832663704,0.0269349931843284)) ;
#12109 = DIRECTION('center_axis',(0.381869435050519,0.921914369154711,-0.0651891902102615)) ;
#12110 = DIRECTION('ref_axis',(0.92421628127522,-0.38091832663704,0.0269349931843284)) ;
#12111 = DIRECTION('center_axis',(-0.921914369154711,-0.381869435050518,0.0651891902102602)) ;
#12112 = DIRECTION('ref_axis',(0.387393722130433,-0.908767745068235,0.155136358012956)) ;
#12113 = DIRECTION('center_axis',(-0.921914369154711,-0.381869435050518,0.0651891902102602)) ;
#12114 = DIRECTION('ref_axis',(0.387393722130433,-0.908767745068235,0.155136358012956)) ;
#12115 = DIRECTION('center_axis',(0.,0.,1.)) ;
#12116 = DIRECTION('ref_axis',(1.,0.,0.)) ;
#12117 = DIRECTION('center_axis',(0.921914369154711,0.381869435050518,-0.0651891902102602)) ;
#12118 = DIRECTION('ref_axis',(0.387393722130433,-0.908767745068235,0.155136358012956)) ;
#12119 = DIRECTION('center_axis',(0.921914369154711,0.381869435050518,-0.0651891902102602)) ;
#12120 = DIRECTION('ref_axis',(0.387393722130433,-0.908767745068235,0.155136358012956)) ;
#12121 = DIRECTION('center_axis',(-0.921914369154711,0.381869435050518,0.065189190210263)) ;
#12122 = DIRECTION('ref_axis',(0.387393722130433,0.908767745068234,0.155136358012963)) ;
#12123 = DIRECTION('center_axis',(0.,0.,1.)) ;
#12124 = DIRECTION('ref_axis',(1.,0.,0.)) ;
#12125 = DIRECTION('center_axis',(0.921914369154711,-0.381869435050518,-0.065189190210263)) ;
#12126 = DIRECTION('ref_axis',(0.387393722130433,0.908767745068234,0.155136358012963)) ;
#12127 = DIRECTION('center_axis',(-0.381869435050518,0.921914369154711,0.0651891902102615)) ;
#12128 = DIRECTION('ref_axis',(0.924216281275221,0.380918326637039,0.0269349931843283)) ;
#12129 = DIRECTION('center_axis',(0.,0.,1.)) ;
#12130 = DIRECTION('ref_axis',(1.,0.,0.)) ;
#12131 = DIRECTION('center_axis',(0.381869435050518,-0.921914369154711,-0.0651891902102615)) ;
#12132 = DIRECTION('ref_axis',(0.924216281275221,0.380918326637039,0.0269349931843283)) ;
#12133 = DIRECTION('center_axis',(0.381869435050518,0.921914369154711,0.0651891902102614)) ;
#12134 = DIRECTION('ref_axis',(0.924216281275221,-0.38091832663704,-0.0269349931843283)) ;
#12135 = DIRECTION('center_axis',(0.,0.,1.)) ;
#12136 = DIRECTION('ref_axis',(1.,0.,0.)) ;
#12137 = DIRECTION('center_axis',(-0.381869435050518,-0.921914369154711,-0.0651891902102614)) ;
#12138 = DIRECTION('ref_axis',(0.924216281275221,-0.38091832663704,-0.0269349931843283)) ;
#12139 = DIRECTION('center_axis',(0.921914369154711,0.381869435050518,0.0651891902102602)) ;
#12140 = DIRECTION('ref_axis',(0.387393722130433,-0.908767745068235,-0.155136358012956)) ;
#12141 = DIRECTION('center_axis',(0.,0.,1.)) ;
#12142 = DIRECTION('ref_axis',(1.,0.,0.)) ;
#12143 = DIRECTION('center_axis',(-0.921914369154711,-0.381869435050518,-0.0651891902102602)) ;
#12144 = DIRECTION('ref_axis',(0.387393722130433,-0.908767745068235,-0.155136358012956)) ;
#12145 = DIRECTION('center_axis',(0.921914369154711,-0.381869435050517,0.0651891902102614)) ;
#12146 = DIRECTION('ref_axis',(0.387393722130433,0.908767745068235,-0.155136358012959)) ;
#12147 = DIRECTION('center_axis',(0.921914369154711,-0.381869435050517,0.0651891902102614)) ;
#12148 = DIRECTION('ref_axis',(0.387393722130433,0.908767745068235,-0.155136358012959)) ;
#12149 = DIRECTION('center_axis',(0.,0.,1.)) ;
#12150 = DIRECTION('ref_axis',(-0.707106781186586,-0.707106781186509,0.)) ;
#12151 = DIRECTION('center_axis',(-0.921914369154711,0.381869435050517,-0.0651891902102614)) ;
#12152 = DIRECTION('ref_axis',(0.387393722130433,0.908767745068235,-0.155136358012959)) ;
#12153 = DIRECTION('center_axis',(-0.921914369154711,0.381869435050517,-0.0651891902102614)) ;
#12154 = DIRECTION('ref_axis',(0.387393722130433,0.908767745068235,-0.155136358012959)) ;
#12155 = DIRECTION('center_axis',(0.381869435050516,-0.921914369154712,0.0651891902102629)) ;
#12156 = DIRECTION('ref_axis',(0.924216281275222,0.380918326637037,-0.0269349931843287)) ;
#12157 = DIRECTION('center_axis',(0.381869435050516,-0.921914369154712,0.0651891902102629)) ;
#12158 = DIRECTION('ref_axis',(0.924216281275222,0.380918326637037,-0.0269349931843287)) ;
#12159 = DIRECTION('center_axis',(0.,0.,1.)) ;
#12160 = DIRECTION('ref_axis',(-1.,-1.55431223447522E-13,0.)) ;
#12161 = DIRECTION('center_axis',(-0.381869435050516,0.921914369154712,-0.0651891902102629)) ;
#12162 = DIRECTION('ref_axis',(0.924216281275222,0.380918326637037,-0.0269349931843287)) ;
#12163 = DIRECTION('center_axis',(-0.381869435050516,0.921914369154712,-0.0651891902102629)) ;
#12164 = DIRECTION('ref_axis',(0.924216281275222,0.380918326637037,-0.0269349931843287)) ;
#12165 = DIRECTION('center_axis',(-0.381869435050519,-0.921914369154711,0.0651891902102608)) ;
#12166 = DIRECTION('ref_axis',(0.92421628127522,-0.38091832663704,0.0269349931843281)) ;
#12167 = DIRECTION('center_axis',(-0.381869435050519,-0.921914369154711,0.0651891902102608)) ;
#12168 = DIRECTION('ref_axis',(0.92421628127522,-0.38091832663704,0.0269349931843281)) ;
#12169 = DIRECTION('center_axis',(0.,0.,1.)) ;
#12170 = DIRECTION('ref_axis',(-0.70710678118647,0.707106781186625,0.)) ;
#12171 = DIRECTION('center_axis',(0.381869435050519,0.921914369154711,-0.0651891902102608)) ;
#12172 = DIRECTION('ref_axis',(0.92421628127522,-0.38091832663704,0.0269349931843281)) ;
#12173 = DIRECTION('center_axis',(0.381869435050519,0.921914369154711,-0.0651891902102608)) ;
#12174 = DIRECTION('ref_axis',(0.92421628127522,-0.38091832663704,0.0269349931843281)) ;
#12175 = DIRECTION('center_axis',(-0.921914369154711,-0.381869435050518,0.0651891902102616)) ;
#12176 = DIRECTION('ref_axis',(0.387393722130434,-0.908767745068234,0.155136358012959)) ;
#12177 = DIRECTION('center_axis',(-0.921914369154711,-0.381869435050518,0.0651891902102616)) ;
#12178 = DIRECTION('ref_axis',(0.387393722130434,-0.908767745068234,0.155136358012959)) ;
#12179 = DIRECTION('center_axis',(0.,0.,1.)) ;
#12180 = DIRECTION('ref_axis',(1.,0.,0.)) ;
#12181 = DIRECTION('center_axis',(0.921914369154711,0.381869435050518,-0.0651891902102616)) ;
#12182 = DIRECTION('ref_axis',(0.387393722130434,-0.908767745068234,0.155136358012959)) ;
#12183 = DIRECTION('center_axis',(0.921914369154711,0.381869435050518,-0.0651891902102616)) ;
#12184 = DIRECTION('ref_axis',(0.387393722130434,-0.908767745068234,0.155136358012959)) ;
#12185 = DIRECTION('center_axis',(-0.921914369154711,0.381869435050518,0.0651891902102608)) ;
#12186 = DIRECTION('ref_axis',(0.387393722130433,0.908767745068235,0.155136358012958)) ;
#12187 = DIRECTION('center_axis',(0.,0.,1.)) ;
#12188 = DIRECTION('ref_axis',(1.,0.,0.)) ;
#12189 = DIRECTION('center_axis',(0.921914369154711,-0.381869435050518,-0.0651891902102608)) ;
#12190 = DIRECTION('ref_axis',(0.387393722130433,0.908767745068235,0.155136358012958)) ;
#12191 = DIRECTION('center_axis',(-0.381869435050518,0.921914369154711,0.0651891902102615)) ;
#12192 = DIRECTION('ref_axis',(0.924216281275221,0.380918326637039,0.0269349931843283)) ;
#12193 = DIRECTION('center_axis',(0.,0.,1.)) ;
#12194 = DIRECTION('ref_axis',(1.,0.,0.)) ;
#12195 = DIRECTION('center_axis',(0.381869435050518,-0.921914369154711,-0.0651891902102615)) ;
#12196 = DIRECTION('ref_axis',(0.924216281275221,0.380918326637039,0.0269349931843283)) ;
#12197 = DIRECTION('center_axis',(0.381869435050517,0.921914369154711,0.0651891902102621)) ;
#12198 = DIRECTION('ref_axis',(0.924216281275221,-0.380918326637038,-0.0269349931843285)) ;
#12199 = DIRECTION('center_axis',(0.,0.,1.)) ;
#12200 = DIRECTION('ref_axis',(1.,0.,0.)) ;
#12201 = DIRECTION('center_axis',(-0.381869435050517,-0.921914369154711,-0.0651891902102621)) ;
#12202 = DIRECTION('ref_axis',(0.924216281275221,-0.380918326637038,-0.0269349931843285)) ;
#12203 = DIRECTION('center_axis',(0.921914369154711,0.381869435050518,0.0651891902102615)) ;
#12204 = DIRECTION('ref_axis',(0.387393722130433,-0.908767745068234,-0.155136358012959)) ;
#12205 = DIRECTION('center_axis',(0.,0.,1.)) ;
#12206 = DIRECTION('ref_axis',(1.,0.,0.)) ;
#12207 = DIRECTION('center_axis',(-0.921914369154711,-0.381869435050518,-0.0651891902102615)) ;
#12208 = DIRECTION('ref_axis',(0.387393722130433,-0.908767745068234,-0.155136358012959)) ;
#12209 = DIRECTION('center_axis',(0.921914369154711,-0.381869435050517,0.0651891902102607)) ;
#12210 = DIRECTION('ref_axis',(0.387393722130432,0.908767745068235,-0.155136358012958)) ;
#12211 = DIRECTION('center_axis',(0.921914369154711,-0.381869435050517,0.0651891902102607)) ;
#12212 = DIRECTION('ref_axis',(0.387393722130432,0.908767745068235,-0.155136358012958)) ;
#12213 = DIRECTION('center_axis',(0.,0.,1.)) ;
#12214 = DIRECTION('ref_axis',(-0.70710678118647,-0.707106781186625,0.)) ;
#12215 = DIRECTION('center_axis',(-0.921914369154711,0.381869435050517,-0.0651891902102607)) ;
#12216 = DIRECTION('ref_axis',(0.387393722130432,0.908767745068235,-0.155136358012958)) ;
#12217 = DIRECTION('center_axis',(-0.921914369154711,0.381869435050517,-0.0651891902102607)) ;
#12218 = DIRECTION('ref_axis',(0.387393722130432,0.908767745068235,-0.155136358012958)) ;
#12219 = DIRECTION('center_axis',(0.381869435050516,-0.921914369154712,0.0651891902102615)) ;
#12220 = DIRECTION('ref_axis',(0.924216281275222,0.380918326637037,-0.0269349931843281)) ;
#12221 = DIRECTION('center_axis',(0.381869435050516,-0.921914369154712,0.0651891902102615)) ;
#12222 = DIRECTION('ref_axis',(0.924216281275222,0.380918326637037,-0.0269349931843281)) ;
#12223 = DIRECTION('center_axis',(0.,0.,1.)) ;
#12224 = DIRECTION('ref_axis',(-1.,7.77156117237609E-14,0.)) ;
#12225 = DIRECTION('center_axis',(-0.381869435050516,0.921914369154712,-0.0651891902102615)) ;
#12226 = DIRECTION('ref_axis',(0.924216281275222,0.380918326637037,-0.0269349931843281)) ;
#12227 = DIRECTION('center_axis',(-0.381869435050516,0.921914369154712,-0.0651891902102615)) ;
#12228 = DIRECTION('ref_axis',(0.924216281275222,0.380918326637037,-0.0269349931843281)) ;
#12229 = DIRECTION('center_axis',(-0.381869435050517,-0.921914369154712,0.0651891902102616)) ;
#12230 = DIRECTION('ref_axis',(0.924216281275221,-0.380918326637038,0.0269349931843282)) ;
#12231 = DIRECTION('center_axis',(-0.381869435050517,-0.921914369154712,0.0651891902102616)) ;
#12232 = DIRECTION('ref_axis',(0.924216281275221,-0.380918326637038,0.0269349931843282)) ;
#12233 = DIRECTION('center_axis',(0.,0.,1.)) ;
#12234 = DIRECTION('ref_axis',(-0.707106781186431,0.707106781186664,0.)) ;
#12235 = DIRECTION('center_axis',(0.381869435050517,0.921914369154712,-0.0651891902102616)) ;
#12236 = DIRECTION('ref_axis',(0.924216281275221,-0.380918326637038,0.0269349931843282)) ;
#12237 = DIRECTION('center_axis',(0.381869435050517,0.921914369154712,-0.0651891902102616)) ;
#12238 = DIRECTION('ref_axis',(0.924216281275221,-0.380918326637038,0.0269349931843282)) ;
#12239 = DIRECTION('center_axis',(-0.921914369154711,-0.381869435050517,0.0651891902102621)) ;
#12240 = DIRECTION('ref_axis',(0.387393722130433,-0.908767745068234,0.155136358012961)) ;
#12241 = DIRECTION('center_axis',(-0.921914369154711,-0.381869435050517,0.0651891902102621)) ;
#12242 = DIRECTION('ref_axis',(0.387393722130433,-0.908767745068234,0.155136358012961)) ;
#12243 = DIRECTION('center_axis',(0.,0.,1.)) ;
#12244 = DIRECTION('ref_axis',(1.,0.,0.)) ;
#12245 = DIRECTION('center_axis',(0.921914369154711,0.381869435050517,-0.0651891902102621)) ;
#12246 = DIRECTION('ref_axis',(0.387393722130433,-0.908767745068234,0.155136358012961)) ;
#12247 = DIRECTION('center_axis',(0.921914369154711,0.381869435050517,-0.0651891902102621)) ;
#12248 = DIRECTION('ref_axis',(0.387393722130433,-0.908767745068234,0.155136358012961)) ;
#12249 = DIRECTION('center_axis',(-0.921914369154711,0.381869435050518,0.0651891902102608)) ;
#12250 = DIRECTION('ref_axis',(0.387393722130433,0.908767745068235,0.155136358012958)) ;
#12251 = DIRECTION('center_axis',(0.,0.,1.)) ;
#12252 = DIRECTION('ref_axis',(1.,0.,0.)) ;
#12253 = DIRECTION('center_axis',(0.921914369154711,-0.381869435050518,-0.0651891902102608)) ;
#12254 = DIRECTION('ref_axis',(0.387393722130433,0.908767745068235,0.155136358012958)) ;
#12255 = DIRECTION('center_axis',(-0.381869435050518,0.921914369154711,0.0651891902102615)) ;
#12256 = DIRECTION('ref_axis',(0.924216281275221,0.380918326637039,0.0269349931843283)) ;
#12257 = DIRECTION('center_axis',(0.381869435050518,0.921914369154711,0.0651891902102614)) ;
#12258 = DIRECTION('ref_axis',(0.924216281275221,-0.38091832663704,-0.0269349931843283)) ;
#12259 = DIRECTION('center_axis',(0.381869435050518,0.921914369154711,0.0651891902102614)) ;
#12260 = DIRECTION('ref_axis',(0.924216281275221,-0.38091832663704,-0.0269349931843283)) ;
#12261 = DIRECTION('',(-0.381869435050518,-0.921914369154711,-0.0651891902102614)) ;
#12262 = DIRECTION('center_axis',(-0.705345615858608,-0.705345615858589,-0.0705345615858606)) ;
#12263 = DIRECTION('ref_axis',(0.707106781186538,-0.707106781186557,1.08220028400547E-15)) ;
#12264 = DIRECTION('center_axis',(-0.705345615858608,-0.705345615858589,-0.0705345615858606)) ;
#12265 = DIRECTION('ref_axis',(0.707106781186538,-0.707106781186557,1.08220028400547E-15)) ;
#12266 = DIRECTION('center_axis',(-0.705345615858608,-0.705345615858589,-0.0705345615858606)) ;
#12267 = DIRECTION('ref_axis',(0.707106781186538,-0.707106781186557,1.08220028400547E-15)) ;
#12268 = DIRECTION('center_axis',(0.381869435050518,0.921914369154711,0.0651891902102614)) ;
#12269 = DIRECTION('ref_axis',(0.924216281275221,-0.38091832663704,-0.0269349931843283)) ;
#12270 = DIRECTION('center_axis',(0.921914369154713,0.381869435050514,0.0651891902102614)) ;
#12271 = DIRECTION('ref_axis',(0.38739372213043,-0.908767745068236,-0.155136358012961)) ;
#12272 = DIRECTION('',(-0.921914369154712,-0.381869435050514,-0.0651891902102614)) ;
#12273 = DIRECTION('center_axis',(-0.997509336107633,-7.23745399280958E-16,
-0.0705345615858551)) ;
#12274 = DIRECTION('ref_axis',(1.43792352550728E-15,-1.,-1.06215953800537E-14)) ;
#12275 = DIRECTION('center_axis',(-0.997509336107633,-7.23745399280958E-16,
-0.0705345615858551)) ;
#12276 = DIRECTION('ref_axis',(1.43792352550728E-15,-1.,-1.06215953800537E-14)) ;
#12277 = DIRECTION('center_axis',(0.921914369154711,-0.381869435050519,0.0651891902102617)) ;
#12278 = DIRECTION('ref_axis',(0.387393722130434,0.908767745068234,-0.155136358012959)) ;
#12279 = DIRECTION('',(-0.921914369154711,0.381869435050519,-0.0651891902102617)) ;
#12280 = DIRECTION('center_axis',(-0.705345615858604,0.705345615858592,-0.0705345615858606)) ;
#12281 = DIRECTION('ref_axis',(0.707106781186541,0.707106781186554,-1.54313744200781E-15)) ;
#12282 = DIRECTION('center_axis',(0.381869435050516,-0.921914369154712,0.0651891902102615)) ;
#12283 = DIRECTION('ref_axis',(0.924216281275222,0.380918326637037,-0.0269349931843281)) ;
#12284 = DIRECTION('',(-0.381869435050516,0.921914369154712,-0.0651891902102615)) ;
#12285 = DIRECTION('center_axis',(0.,0.997509336107633,-0.0705345615858551)) ;
#12286 = DIRECTION('ref_axis',(1.,0.,0.)) ;
#12287 = DIRECTION('center_axis',(-0.381869435050518,-0.921914369154711,0.0651891902102613)) ;
#12288 = DIRECTION('ref_axis',(0.924216281275221,-0.380918326637039,0.0269349931843282)) ;
#12289 = DIRECTION('',(0.381869435050518,0.921914369154711,-0.0651891902102613)) ;
#12290 = DIRECTION('center_axis',(0.705345615858603,0.705345615858593,-0.0705345615858606)) ;
#12291 = DIRECTION('ref_axis',(0.707106781186542,-0.707106781186553,-1.76358564800892E-15)) ;
#12292 = DIRECTION('center_axis',(-0.921914369154711,-0.381869435050517,0.0651891902102618)) ;
#12293 = DIRECTION('ref_axis',(0.387393722130432,-0.908767745068235,0.15513635801296)) ;
#12294 = DIRECTION('',(0.921914369154711,0.381869435050517,-0.0651891902102618)) ;
#12295 = DIRECTION('center_axis',(0.997509336107633,-1.02353055936833E-14,
-0.0705345615858551)) ;
#12296 = DIRECTION('ref_axis',(-9.27636030479688E-15,-1.,1.27859959480646E-14)) ;
#12297 = DIRECTION('center_axis',(0.997509336107633,-1.02353055936833E-14,
-0.0705345615858551)) ;
#12298 = DIRECTION('ref_axis',(-9.27636030479688E-15,-1.,1.27859959480646E-14)) ;
#12299 = DIRECTION('center_axis',(-0.921914369154711,0.381869435050517,0.0651891902102614)) ;
#12300 = DIRECTION('ref_axis',(0.387393722130432,0.908767745068235,0.155136358012959)) ;
#12301 = DIRECTION('',(0.921914369154711,-0.381869435050517,-0.0651891902102613)) ;
#12302 = DIRECTION('center_axis',(0.705345615858604,-0.705345615858593,-0.0705345615858606)) ;
#12303 = DIRECTION('ref_axis',(0.707106781186542,0.707106781186553,2.56521548801298E-15)) ;
#12304 = DIRECTION('center_axis',(0.705345615858604,-0.705345615858593,-0.0705345615858606)) ;
#12305 = DIRECTION('ref_axis',(0.707106781186542,0.707106781186553,2.56521548801298E-15)) ;
#12306 = DIRECTION('center_axis',(0.705345615858604,-0.705345615858593,-0.0705345615858606)) ;
#12307 = DIRECTION('ref_axis',(0.707106781186542,0.707106781186553,2.56521548801298E-15)) ;
#12308 = DIRECTION('center_axis',(-0.381869435050518,0.921914369154711,0.0651891902102615)) ;
#12309 = DIRECTION('ref_axis',(0.924216281275221,0.380918326637039,0.0269349931843283)) ;
#12310 = DIRECTION('',(0.381869435050518,-0.921914369154711,-0.0651891902102615)) ;
#12311 = DIRECTION('center_axis',(-1.02353055936834E-14,-0.997509336107633,
-0.0705345615858551)) ;
#12312 = DIRECTION('ref_axis',(1.,-1.01806989680515E-14,-7.16456669503621E-16)) ;
#12313 = DIRECTION('center_axis',(-1.02353055936834E-14,-0.997509336107633,
-0.0705345615858551)) ;
#12314 = DIRECTION('ref_axis',(1.,-1.01806989680515E-14,-7.16456669503621E-16)) ;
#12315 = DIRECTION('center_axis',(0.381869435050518,0.921914369154711,0.0651891902102614)) ;
#12316 = DIRECTION('ref_axis',(0.924216281275221,-0.38091832663704,-0.0269349931843283)) ;
#12317 = DIRECTION('',(-0.381869435050518,-0.921914369154711,-0.0651891902102614)) ;
#12318 = DIRECTION('center_axis',(-0.705345615858608,-0.705345615858589,-0.0705345615858606)) ;
#12319 = DIRECTION('ref_axis',(0.707106781186538,-0.707106781186557,1.08220028400547E-15)) ;
#12320 = DIRECTION('center_axis',(-0.705345615858608,-0.705345615858589,-0.0705345615858606)) ;
#12321 = DIRECTION('ref_axis',(0.707106781186538,-0.707106781186557,1.08220028400547E-15)) ;
#12322 = DIRECTION('center_axis',(-0.705345615858608,-0.705345615858589,-0.0705345615858606)) ;
#12323 = DIRECTION('ref_axis',(0.707106781186538,-0.707106781186557,1.08220028400547E-15)) ;
#12324 = DIRECTION('center_axis',(0.921914369154711,0.381869435050517,0.0651891902102614)) ;
#12325 = DIRECTION('ref_axis',(0.387393722130433,-0.908767745068235,-0.155136358012959)) ;
#12326 = DIRECTION('',(-0.921914369154711,-0.381869435050517,-0.0651891902102614)) ;
#12327 = DIRECTION('center_axis',(-0.997509336107633,-1.44749079856192E-15,
-0.0705345615858551)) ;
#12328 = DIRECTION('ref_axis',(2.24706864526137E-15,-1.,-1.05815138880535E-14)) ;
#12329 = DIRECTION('center_axis',(-0.997509336107633,-1.44749079856192E-15,
-0.0705345615858551)) ;
#12330 = DIRECTION('ref_axis',(2.24706864526137E-15,-1.,-1.05815138880535E-14)) ;
#12331 = DIRECTION('center_axis',(0.921914369154711,-0.381869435050518,0.0651891902102616)) ;
#12332 = DIRECTION('ref_axis',(0.387393722130434,0.908767745068234,-0.155136358012959)) ;
#12333 = DIRECTION('',(-0.921914369154711,0.381869435050518,-0.0651891902102616)) ;
#12334 = DIRECTION('center_axis',(-0.705345615858604,0.705345615858592,-0.0705345615858606)) ;
#12335 = DIRECTION('ref_axis',(0.707106781186541,0.707106781186554,-1.60325968000812E-15)) ;
#12336 = DIRECTION('center_axis',(0.381869435050516,-0.921914369154712,0.0651891902102615)) ;
#12337 = DIRECTION('ref_axis',(0.924216281275222,0.380918326637037,-0.0269349931843281)) ;
#12338 = DIRECTION('',(-0.381869435050516,0.921914369154712,-0.0651891902102615)) ;
#12339 = DIRECTION('center_axis',(1.02353055936834E-14,0.997509336107633,
-0.0705345615858551)) ;
#12340 = DIRECTION('ref_axis',(1.,-1.02207804600517E-14,7.21466856003647E-16)) ;
#12341 = DIRECTION('center_axis',(-0.381869435050519,-0.921914369154711,0.0651891902102615)) ;
#12342 = DIRECTION('ref_axis',(0.92421628127522,-0.38091832663704,0.0269349931843284)) ;
#12343 = DIRECTION('',(0.381869435050519,0.92191436915471,-0.0651891902102615)) ;
#12344 = DIRECTION('center_axis',(0.705345615858598,0.705345615858598,-0.0705345615858606)) ;
#12345 = DIRECTION('ref_axis',(0.707106781186547,-0.707106781186548,-1.79364676700907E-15)) ;
#12346 = DIRECTION('center_axis',(-0.921914369154711,-0.381869435050518,0.0651891902102602)) ;
#12347 = DIRECTION('ref_axis',(0.387393722130433,-0.908767745068235,0.155136358012956)) ;
#12348 = DIRECTION('',(0.921914369154711,0.381869435050518,-0.0651891902102602)) ;
#12349 = DIRECTION('center_axis',(0.997509336107633,-1.09590509929644E-14,
-0.0705345615858551)) ;
#12350 = DIRECTION('ref_axis',(-1.03861166145525E-14,-1.,8.47723555804284E-15)) ;
#12351 = DIRECTION('center_axis',(0.997509336107633,-1.09590509929644E-14,
-0.0705345615858551)) ;
#12352 = DIRECTION('ref_axis',(-1.03861166145525E-14,-1.,8.47723555804284E-15)) ;
#12353 = DIRECTION('center_axis',(-0.921914369154711,0.381869435050518,0.065189190210263)) ;
#12354 = DIRECTION('ref_axis',(0.387393722130433,0.908767745068234,0.155136358012963)) ;
#12355 = DIRECTION('',(0.921914369154711,-0.381869435050518,-0.065189190210263)) ;
#12356 = DIRECTION('center_axis',(0.705345615858598,-0.705345615858599,-0.0705345615858606)) ;
#12357 = DIRECTION('ref_axis',(0.707106781186548,0.707106781186547,-2.20448206001115E-15)) ;
#12358 = DIRECTION('center_axis',(0.705345615858598,-0.705345615858599,-0.0705345615858606)) ;
#12359 = DIRECTION('ref_axis',(0.707106781186548,0.707106781186547,-2.20448206001115E-15)) ;
#12360 = DIRECTION('center_axis',(0.705345615858598,-0.705345615858599,-0.0705345615858606)) ;
#12361 = DIRECTION('ref_axis',(0.707106781186548,0.707106781186547,-2.20448206001115E-15)) ;
#12362 = DIRECTION('center_axis',(-0.381869435050518,0.921914369154711,0.0651891902102615)) ;
#12363 = DIRECTION('ref_axis',(0.924216281275221,0.380918326637039,0.0269349931843283)) ;
#12364 = DIRECTION('',(0.381869435050518,-0.921914369154711,-0.0651891902102615)) ;
#12365 = DIRECTION('center_axis',(-1.02353055936834E-14,-0.997509336107633,
-0.0705345615858551)) ;
#12366 = DIRECTION('ref_axis',(1.,-1.01806989680515E-14,-7.16456669503621E-16)) ;
#12367 = DIRECTION('center_axis',(-1.02353055936834E-14,-0.997509336107633,
-0.0705345615858551)) ;
#12368 = DIRECTION('ref_axis',(1.,-1.01806989680515E-14,-7.16456669503621E-16)) ;
#12369 = DIRECTION('center_axis',(0.381869435050518,0.921914369154711,0.0651891902102614)) ;
#12370 = DIRECTION('ref_axis',(0.924216281275221,-0.38091832663704,-0.0269349931843283)) ;
#12371 = DIRECTION('',(-0.381869435050518,-0.921914369154711,-0.0651891902102614)) ;
#12372 = DIRECTION('center_axis',(-0.705345615858604,-0.705345615858593,-0.0705345615858606)) ;
#12373 = DIRECTION('ref_axis',(0.707106781186542,-0.707106781186553,1.5631781880079E-15)) ;
#12374 = DIRECTION('center_axis',(-0.705345615858604,-0.705345615858593,-0.0705345615858606)) ;
#12375 = DIRECTION('ref_axis',(0.707106781186542,-0.707106781186553,1.5631781880079E-15)) ;
#12376 = DIRECTION('center_axis',(-0.705345615858604,-0.705345615858593,-0.0705345615858606)) ;
#12377 = DIRECTION('ref_axis',(0.707106781186542,-0.707106781186553,1.5631781880079E-15)) ;
#12378 = DIRECTION('center_axis',(0.921914369154711,0.381869435050518,0.0651891902102602)) ;
#12379 = DIRECTION('ref_axis',(0.387393722130433,-0.908767745068235,-0.155136358012956)) ;
#12380 = DIRECTION('',(-0.921914369154711,-0.381869435050518,-0.0651891902102602)) ;
#12381 = DIRECTION('center_axis',(-0.997509336107633,1.02353055936834E-14,
-0.0705345615858551)) ;
#12382 = DIRECTION('ref_axis',(-9.60953770704856E-15,-1.,-8.47723555804284E-15)) ;
#12383 = DIRECTION('center_axis',(-0.997509336107633,1.02353055936834E-14,
-0.0705345615858551)) ;
#12384 = DIRECTION('ref_axis',(-9.60953770704856E-15,-1.,-8.47723555804284E-15)) ;
#12385 = DIRECTION('center_axis',(0.921914369154711,-0.381869435050517,0.0651891902102614)) ;
#12386 = DIRECTION('ref_axis',(0.387393722130433,0.908767745068235,-0.155136358012959)) ;
#12387 = DIRECTION('',(-0.921914369154711,0.381869435050517,-0.0651891902102614)) ;
#12388 = DIRECTION('center_axis',(-0.705345615858599,0.705345615858598,-0.070534561585861)) ;
#12389 = DIRECTION('ref_axis',(0.707106781186547,0.707106781186548,-2.50509325001267E-15)) ;
#12390 = DIRECTION('center_axis',(0.381869435050516,-0.921914369154712,0.0651891902102629)) ;
#12391 = DIRECTION('ref_axis',(0.924216281275222,0.380918326637037,-0.0269349931843287)) ;
#12392 = DIRECTION('',(-0.381869435050516,0.921914369154712,-0.0651891902102629)) ;
#12393 = DIRECTION('center_axis',(1.02353055936834E-14,0.997509336107633,
-0.0705345615858553)) ;
#12394 = DIRECTION('ref_axis',(1.,-1.02207804600517E-14,7.31487229003697E-16)) ;
#12395 = DIRECTION('center_axis',(-0.381869435050519,-0.921914369154711,0.0651891902102608)) ;
#12396 = DIRECTION('ref_axis',(0.92421628127522,-0.38091832663704,0.0269349931843281)) ;
#12397 = DIRECTION('',(0.381869435050519,0.92191436915471,-0.0651891902102608)) ;
#12398 = DIRECTION('center_axis',(0.705345615858598,0.705345615858598,-0.0705345615858606)) ;
#12399 = DIRECTION('ref_axis',(0.707106781186547,-0.707106781186548,-3.78770099401916E-15)) ;
#12400 = DIRECTION('center_axis',(-0.921914369154711,-0.381869435050518,0.0651891902102616)) ;
#12401 = DIRECTION('ref_axis',(0.387393722130434,-0.908767745068234,0.155136358012959)) ;
#12402 = DIRECTION('',(0.921914369154711,0.381869435050518,-0.0651891902102616)) ;
#12403 = DIRECTION('center_axis',(0.997509336107633,-7.2374539928096E-16,
-0.0705345615858553)) ;
#12404 = DIRECTION('ref_axis',(1.42790315250722E-16,-1.,1.09422473160553E-14)) ;
#12405 = DIRECTION('center_axis',(0.997509336107633,-7.2374539928096E-16,
-0.0705345615858553)) ;
#12406 = DIRECTION('ref_axis',(1.42790315250722E-16,-1.,1.09422473160553E-14)) ;
#12407 = DIRECTION('center_axis',(-0.921914369154711,0.381869435050518,0.0651891902102608)) ;
#12408 = DIRECTION('ref_axis',(0.387393722130433,0.908767745068235,0.155136358012958)) ;
#12409 = DIRECTION('',(0.921914369154711,-0.381869435050518,-0.0651891902102608)) ;
#12410 = DIRECTION('center_axis',(0.705345615858603,-0.705345615858593,-0.070534561585861)) ;
#12411 = DIRECTION('ref_axis',(0.707106781186543,0.707106781186552,4.90998277002485E-15)) ;
#12412 = DIRECTION('center_axis',(0.705345615858603,-0.705345615858593,-0.070534561585861)) ;
#12413 = DIRECTION('ref_axis',(0.707106781186543,0.707106781186552,4.90998277002485E-15)) ;
#12414 = DIRECTION('center_axis',(0.705345615858603,-0.705345615858593,-0.070534561585861)) ;
#12415 = DIRECTION('ref_axis',(0.707106781186543,0.707106781186552,4.90998277002485E-15)) ;
#12416 = DIRECTION('center_axis',(-0.381869435050518,0.921914369154711,0.0651891902102615)) ;
#12417 = DIRECTION('ref_axis',(0.924216281275221,0.380918326637039,0.0269349931843283)) ;
#12418 = DIRECTION('',(0.381869435050518,-0.921914369154711,-0.0651891902102615)) ;
#12419 = DIRECTION('center_axis',(0.,-0.997509336107633,-0.0705345615858555)) ;
#12420 = DIRECTION('ref_axis',(1.,4.00814920002027E-17,5.01018650002534E-18)) ;
#12421 = DIRECTION('center_axis',(0.,-0.997509336107633,-0.0705345615858555)) ;
#12422 = DIRECTION('ref_axis',(1.,4.00814920002027E-17,5.01018650002534E-18)) ;
#12423 = DIRECTION('center_axis',(0.381869435050517,0.921914369154711,0.0651891902102621)) ;
#12424 = DIRECTION('ref_axis',(0.924216281275221,-0.380918326637038,-0.0269349931843285)) ;
#12425 = DIRECTION('',(-0.381869435050517,-0.921914369154711,-0.0651891902102621)) ;
#12426 = DIRECTION('center_axis',(-0.705345615858593,-0.705345615858604,-0.070534561585861)) ;
#12427 = DIRECTION('ref_axis',(0.707106781186553,-0.707106781186542,1.43291333900725E-15)) ;
#12428 = DIRECTION('center_axis',(-0.705345615858593,-0.705345615858604,-0.070534561585861)) ;
#12429 = DIRECTION('ref_axis',(0.707106781186553,-0.707106781186542,1.43291333900725E-15)) ;
#12430 = DIRECTION('center_axis',(-0.705345615858593,-0.705345615858604,-0.070534561585861)) ;
#12431 = DIRECTION('ref_axis',(0.707106781186553,-0.707106781186542,1.43291333900725E-15)) ;
#12432 = DIRECTION('center_axis',(0.921914369154711,0.381869435050518,0.0651891902102615)) ;
#12433 = DIRECTION('ref_axis',(0.387393722130433,-0.908767745068234,-0.155136358012959)) ;
#12434 = DIRECTION('',(-0.921914369154711,-0.381869435050518,-0.0651891902102615)) ;
#12435 = DIRECTION('center_axis',(-0.997509336107633,3.61872699640481E-16,
-0.0705345615858555)) ;
#12436 = DIRECTION('ref_axis',(4.65947344502357E-16,-1.,-1.07217991100542E-14)) ;
#12437 = DIRECTION('center_axis',(-0.997509336107633,3.61872699640481E-16,
-0.0705345615858555)) ;
#12438 = DIRECTION('ref_axis',(4.65947344502357E-16,-1.,-1.07217991100542E-14)) ;
#12439 = DIRECTION('center_axis',(0.921914369154711,-0.381869435050517,0.0651891902102607)) ;
#12440 = DIRECTION('ref_axis',(0.387393722130432,0.908767745068235,-0.155136358012958)) ;
#12441 = DIRECTION('',(-0.921914369154711,0.381869435050517,-0.0651891902102607)) ;
#12442 = DIRECTION('center_axis',(-0.705345615858603,0.705345615858593,-0.070534561585861)) ;
#12443 = DIRECTION('ref_axis',(0.707106781186543,0.707106781186552,-5.17051246802617E-15)) ;
#12444 = DIRECTION('center_axis',(0.381869435050516,-0.921914369154712,0.0651891902102615)) ;
#12445 = DIRECTION('ref_axis',(0.924216281275222,0.380918326637037,-0.0269349931843281)) ;
#12446 = DIRECTION('',(-0.381869435050516,0.921914369154712,-0.0651891902102615)) ;
#12447 = DIRECTION('center_axis',(0.,0.997509336107633,-0.0705345615858555)) ;
#12448 = DIRECTION('ref_axis',(1.,0.,0.)) ;
#12449 = DIRECTION('center_axis',(-0.381869435050517,-0.921914369154712,0.0651891902102616)) ;
#12450 = DIRECTION('ref_axis',(0.924216281275221,-0.380918326637038,0.0269349931843282)) ;
#12451 = DIRECTION('',(0.381869435050517,0.921914369154711,-0.0651891902102615)) ;
#12452 = DIRECTION('center_axis',(0.705345615858583,0.705345615858614,-0.070534561585861)) ;
#12453 = DIRECTION('ref_axis',(0.707106781186563,-0.707106781186532,-4.02818994602041E-15)) ;
#12454 = DIRECTION('center_axis',(-0.921914369154711,-0.381869435050517,0.0651891902102621)) ;
#12455 = DIRECTION('ref_axis',(0.387393722130433,-0.908767745068234,0.155136358012961)) ;
#12456 = DIRECTION('',(0.921914369154711,0.381869435050517,-0.0651891902102621)) ;
#12457 = DIRECTION('center_axis',(0.997509336107633,-9.87343289404283E-15,
-0.0705345615858555)) ;
#12458 = DIRECTION('ref_axis',(-8.91312178354505E-15,-1.,1.31667701220665E-14)) ;
#12459 = DIRECTION('center_axis',(0.997509336107633,-9.87343289404283E-15,
-0.0705345615858555)) ;
#12460 = DIRECTION('ref_axis',(-8.91312178354505E-15,-1.,1.31667701220665E-14)) ;
#12461 = DIRECTION('center_axis',(-0.921914369154711,0.381869435050518,0.0651891902102608)) ;
#12462 = DIRECTION('ref_axis',(0.387393722130433,0.908767745068235,0.155136358012958)) ;
#12463 = DIRECTION('',(0.921914369154711,-0.381869435050518,-0.0651891902102608)) ;
#12464 = DIRECTION('center_axis',(0.705345615858603,-0.705345615858593,-0.070534561585861)) ;
#12465 = DIRECTION('ref_axis',(0.707106781186543,0.707106781186552,4.90998277002485E-15)) ;
#12466 = DIRECTION('center_axis',(0.705345615858603,-0.705345615858593,-0.070534561585861)) ;
#12467 = DIRECTION('ref_axis',(0.707106781186543,0.707106781186552,4.90998277002485E-15)) ;
#12468 = DIRECTION('center_axis',(0.705345615858603,-0.705345615858593,-0.070534561585861)) ;
#12469 = DIRECTION('ref_axis',(0.707106781186543,0.707106781186552,4.90998277002485E-15)) ;
#12470 = DIRECTION('center_axis',(-0.381869435050518,0.921914369154711,0.0651891902102615)) ;
#12471 = DIRECTION('ref_axis',(0.924216281275221,0.380918326637039,0.0269349931843283)) ;
#12472 = DIRECTION('',(0.381869435050518,-0.921914369154711,-0.0651891902102615)) ;
#12473 = DIRECTION('center_axis',(0.381869435050518,-0.921914369154711,-0.0651891902102615)) ;
#12474 = DIRECTION('ref_axis',(0.924216281275221,0.380918326637039,0.0269349931843283)) ;
#12475 = DIRECTION('center_axis',(0.381869435050518,-0.921914369154711,-0.0651891902102615)) ;
#12476 = DIRECTION('ref_axis',(-0.924216281275221,-0.380918326637039,-0.0269349931843283)) ;
#12477 = DIRECTION('',(0.,0.,1.)) ;
#12478 = DIRECTION('',(1.,0.,0.)) ;
#12479 = DIRECTION('',(0.,0.,1.)) ;
#12480 = DIRECTION('',(1.,0.,0.)) ;
#12481 = DIRECTION('',(0.,0.,1.)) ;
#12482 = DIRECTION('',(1.,0.,0.)) ;
#12483 = DIRECTION('',(0.,0.,1.)) ;
#12484 = DIRECTION('',(1.,0.,0.)) ;
#12485 = DIRECTION('',(0.,0.,1.)) ;
#12486 = DIRECTION('',(1.,0.,0.)) ;
#12487 = DIRECTION('',(0.,0.,1.)) ;
#12488 = DIRECTION('',(1.,0.,0.)) ;
#12489 = DIRECTION('',(0.,0.,1.)) ;
#12490 = DIRECTION('',(1.,0.,0.)) ;
#12491 = DIRECTION('',(0.,0.,1.)) ;
#12492 = DIRECTION('',(1.,0.,0.)) ;
#12493 = DIRECTION('',(0.,0.,1.)) ;
#12494 = DIRECTION('',(1.,0.,0.)) ;
#12495 = DIRECTION('',(0.,0.,1.)) ;
#12496 = DIRECTION('',(1.,0.,0.)) ;
#12497 = DIRECTION('',(0.,0.,1.)) ;
#12498 = DIRECTION('',(1.,0.,0.)) ;
#12499 = DIRECTION('axis',(0.,0.,1.)) ;
#12500 = DIRECTION('refdir',(1.,0.,0.)) ;
#12501 = DIRECTION('axis',(0.,0.,1.)) ;
#12502 = DIRECTION('refdir',(1.,0.,0.)) ;
#12503 = DIRECTION('center_axis',(1.,0.,0.)) ;
#12504 = DIRECTION('ref_axis',(0.,0.,-1.)) ;
#12505 = DIRECTION('center_axis',(1.,0.,0.)) ;
#12506 = DIRECTION('ref_axis',(0.,0.,-1.)) ;
#12507 = DIRECTION('',(1.,0.,0.)) ;
#12508 = DIRECTION('center_axis',(-1.,0.,0.)) ;
#12509 = DIRECTION('ref_axis',(0.,0.,-1.)) ;
#12510 = DIRECTION('center_axis',(1.,0.,0.)) ;
#12511 = DIRECTION('ref_axis',(0.,0.,-1.)) ;
#12512 = DIRECTION('',(0.,1.,0.)) ;
#12513 = DIRECTION('',(0.,0.,-1.)) ;
#12514 = DIRECTION('',(0.,-1.,0.)) ;
#12515 = DIRECTION('',(0.,0.,-1.)) ;
#12516 = DIRECTION('center_axis',(0.,0.,1.)) ;
#12517 = DIRECTION('ref_axis',(1.,0.,0.)) ;
#12518 = DIRECTION('',(0.,1.,0.)) ;
#12519 = DIRECTION('',(-1.,0.,0.)) ;
#12520 = DIRECTION('',(1.,0.,0.)) ;
#12521 = DIRECTION('center_axis',(-1.,0.,0.)) ;
#12522 = DIRECTION('ref_axis',(0.,0.,1.)) ;
#12523 = DIRECTION('',(0.,-1.,0.)) ;
#12524 = DIRECTION('',(0.,0.,-1.)) ;
#12525 = DIRECTION('',(0.,0.,-1.)) ;
#12526 = DIRECTION('center_axis',(0.,0.,1.)) ;
#12527 = DIRECTION('ref_axis',(1.,0.,0.)) ;
#12528 = DIRECTION('',(1.,0.,0.)) ;
#12529 = DIRECTION('',(0.,-1.,0.)) ;
#12530 = DIRECTION('',(-1.,0.,0.)) ;
#12531 = DIRECTION('',(0.,1.,0.)) ;
#12532 = DIRECTION('center_axis',(0.,0.,1.)) ;
#12533 = DIRECTION('ref_axis',(1.,0.,0.)) ;
#12534 = DIRECTION('',(1.,0.,0.)) ;
#12535 = DIRECTION('',(0.,1.,0.)) ;
#12536 = DIRECTION('',(-1.,0.,0.)) ;
#12537 = DIRECTION('center_axis',(0.,0.,1.)) ;
#12538 = DIRECTION('ref_axis',(1.,0.,0.)) ;
#12539 = DIRECTION('',(-1.,0.,0.)) ;
#12540 = DIRECTION('',(0.,-1.,0.)) ;
#12541 = DIRECTION('',(1.,0.,0.)) ;
#12542 = DIRECTION('center_axis',(0.,1.,0.)) ;
#12543 = DIRECTION('ref_axis',(0.,0.,1.)) ;
#12544 = DIRECTION('',(0.,0.,-1.)) ;
#12545 = DIRECTION('',(0.,0.,-1.)) ;
#12546 = DIRECTION('center_axis',(1.,0.,0.)) ;
#12547 = DIRECTION('ref_axis',(0.,0.,-1.)) ;
#12548 = DIRECTION('',(0.,0.,-1.)) ;
#12549 = DIRECTION('center_axis',(0.,-1.,0.)) ;
#12550 = DIRECTION('ref_axis',(0.,0.,-1.)) ;
#12551 = DIRECTION('',(0.,0.,-1.)) ;
#12552 = DIRECTION('center_axis',(-1.,0.,0.)) ;
#12553 = DIRECTION('ref_axis',(0.,0.,1.)) ;
#12554 = DIRECTION('axis',(0.,0.,1.)) ;
#12555 = DIRECTION('refdir',(1.,0.,0.)) ;
#12556 = DIRECTION('center_axis',(0.,0.,1.)) ;
#12557 = DIRECTION('ref_axis',(1.,0.,0.)) ;
#12558 = DIRECTION('',(0.,-1.,0.)) ;
#12559 = DIRECTION('',(-1.,0.,0.)) ;
#12560 = DIRECTION('',(0.,1.,0.)) ;
#12561 = DIRECTION('',(1.,0.,0.)) ;
#12562 = DIRECTION('center_axis',(0.,1.,0.)) ;
#12563 = DIRECTION('ref_axis',(0.,0.,1.)) ;
#12564 = DIRECTION('',(0.,0.,-1.)) ;
#12565 = DIRECTION('',(0.,0.,-1.)) ;
#12566 = DIRECTION('',(-1.,0.,0.)) ;
#12567 = DIRECTION('center_axis',(0.,0.,1.)) ;
#12568 = DIRECTION('ref_axis',(1.,0.,0.)) ;
#12569 = DIRECTION('',(0.,1.,0.)) ;
#12570 = DIRECTION('',(0.,-1.,0.)) ;
#12571 = DIRECTION('',(1.,0.,0.)) ;
#12572 = DIRECTION('center_axis',(0.,-1.,0.)) ;
#12573 = DIRECTION('ref_axis',(0.,0.,-1.)) ;
#12574 = DIRECTION('',(0.,0.,1.)) ;
#12575 = DIRECTION('',(0.,0.,-1.)) ;
#12576 = DIRECTION('center_axis',(-1.,0.,0.)) ;
#12577 = DIRECTION('ref_axis',(0.,0.,1.)) ;
#12578 = DIRECTION('center_axis',(-1.,0.,0.)) ;
#12579 = DIRECTION('ref_axis',(0.,0.,-1.)) ;
#12580 = DIRECTION('center_axis',(1.,0.,0.)) ;
#12581 = DIRECTION('ref_axis',(0.,0.,-1.)) ;
#12582 = DIRECTION('',(1.,0.,0.)) ;
#12583 = DIRECTION('center_axis',(-1.,0.,0.)) ;
#12584 = DIRECTION('ref_axis',(0.,0.,-1.)) ;
#12585 = DIRECTION('center_axis',(0.,0.,1.)) ;
#12586 = DIRECTION('ref_axis',(1.,0.,0.)) ;
#12587 = DIRECTION('',(0.,1.,0.)) ;
#12588 = DIRECTION('',(-1.,0.,0.)) ;
#12589 = DIRECTION('',(0.,-1.,0.)) ;
#12590 = DIRECTION('',(1.,0.,0.)) ;
#12591 = DIRECTION('center_axis',(0.,0.,1.)) ;
#12592 = DIRECTION('ref_axis',(1.,0.,0.)) ;
#12593 = DIRECTION('',(0.,-1.,0.)) ;
#12594 = DIRECTION('',(-1.,0.,0.)) ;
#12595 = DIRECTION('',(0.,1.,0.)) ;
#12596 = DIRECTION('',(1.,0.,0.)) ;
#12597 = DIRECTION('center_axis',(0.,1.,0.)) ;
#12598 = DIRECTION('ref_axis',(0.,0.,1.)) ;
#12599 = DIRECTION('',(0.,0.,-1.)) ;
#12600 = DIRECTION('',(0.,0.,-1.)) ;
#12601 = DIRECTION('center_axis',(1.,0.,0.)) ;
#12602 = DIRECTION('ref_axis',(0.,0.,-1.)) ;
#12603 = DIRECTION('',(0.,0.,-1.)) ;
#12604 = DIRECTION('center_axis',(0.,-1.,0.)) ;
#12605 = DIRECTION('ref_axis',(0.,0.,-1.)) ;
#12606 = DIRECTION('',(0.,0.,-1.)) ;
#12607 = DIRECTION('center_axis',(-1.,0.,0.)) ;
#12608 = DIRECTION('ref_axis',(0.,0.,1.)) ;
#12609 = DIRECTION('axis',(0.,0.,1.)) ;
#12610 = DIRECTION('refdir',(1.,0.,0.)) ;
#12611 = DIRECTION('center_axis',(0.,0.,1.)) ;
#12612 = DIRECTION('ref_axis',(1.,0.,0.)) ;
#12613 = DIRECTION('center_axis',(0.,-1.,0.)) ;
#12614 = DIRECTION('ref_axis',(-1.,0.,0.)) ;
#12615 = DIRECTION('center_axis',(-1.,0.,0.)) ;
#12616 = DIRECTION('ref_axis',(0.,0.,-1.)) ;
#12617 = DIRECTION('center_axis',(0.,0.,1.)) ;
#12618 = DIRECTION('ref_axis',(1.,0.,0.)) ;
#12619 = DIRECTION('center_axis',(-1.,0.,0.)) ;
#12620 = DIRECTION('ref_axis',(0.,0.,-1.)) ;
#12621 = DIRECTION('center_axis',(1.,0.,0.)) ;
#12622 = DIRECTION('ref_axis',(0.,0.,-1.)) ;
#12623 = DIRECTION('center_axis',(1.,0.,0.)) ;
#12624 = DIRECTION('ref_axis',(0.,0.,-1.)) ;
#12625 = DIRECTION('',(-1.,0.,0.)) ;
#12626 = DIRECTION('center_axis',(1.,0.,0.)) ;
#12627 = DIRECTION('ref_axis',(0.,0.,-1.)) ;
#12628 = DIRECTION('center_axis',(1.,0.,0.)) ;
#12629 = DIRECTION('ref_axis',(0.,0.,-1.)) ;
#12630 = DIRECTION('center_axis',(1.,0.,0.)) ;
#12631 = DIRECTION('ref_axis',(0.,0.,-1.)) ;
#12632 = DIRECTION('',(-1.,0.,0.)) ;
#12633 = DIRECTION('center_axis',(-1.,0.,0.)) ;
#12634 = DIRECTION('ref_axis',(0.,0.,-1.)) ;
#12635 = DIRECTION('center_axis',(-1.,0.,0.)) ;
#12636 = DIRECTION('ref_axis',(0.,0.,1.)) ;
#12637 = DIRECTION('center_axis',(1.,0.,0.)) ;
#12638 = DIRECTION('ref_axis',(0.,0.,-1.)) ;
#12639 = DIRECTION('center_axis',(1.,0.,0.)) ;
#12640 = DIRECTION('ref_axis',(0.,0.,-1.)) ;
#12641 = DIRECTION('center_axis',(1.,0.,0.)) ;
#12642 = DIRECTION('ref_axis',(0.,0.,-1.)) ;
#12643 = DIRECTION('',(-1.,0.,0.)) ;
#12644 = DIRECTION('center_axis',(-1.,0.,0.)) ;
#12645 = DIRECTION('ref_axis',(0.,0.,-1.)) ;
#12646 = DIRECTION('center_axis',(-1.,0.,0.)) ;
#12647 = DIRECTION('ref_axis',(0.,0.,1.)) ;
#12648 = DIRECTION('center_axis',(1.,0.,0.)) ;
#12649 = DIRECTION('ref_axis',(0.,0.,-1.)) ;
#12650 = DIRECTION('axis',(0.,0.,1.)) ;
#12651 = DIRECTION('refdir',(1.,0.,0.)) ;
#12652 = DIRECTION('center_axis',(1.,0.,0.)) ;
#12653 = DIRECTION('ref_axis',(0.,0.,-1.)) ;
#12654 = DIRECTION('center_axis',(1.,0.,0.)) ;
#12655 = DIRECTION('ref_axis',(0.,0.,-1.)) ;
#12656 = DIRECTION('',(-1.,0.,0.)) ;
#12657 = DIRECTION('center_axis',(-1.,0.,0.)) ;
#12658 = DIRECTION('ref_axis',(0.,0.,-1.)) ;
#12659 = DIRECTION('center_axis',(-1.,0.,0.)) ;
#12660 = DIRECTION('ref_axis',(0.,0.,1.)) ;
#12661 = DIRECTION('center_axis',(1.,0.,0.)) ;
#12662 = DIRECTION('ref_axis',(0.,0.,-1.)) ;
#12663 = DIRECTION('center_axis',(1.,0.,0.)) ;
#12664 = DIRECTION('ref_axis',(0.,0.,-1.)) ;
#12665 = DIRECTION('center_axis',(1.,0.,0.)) ;
#12666 = DIRECTION('ref_axis',(0.,0.,-1.)) ;
#12667 = DIRECTION('',(-1.,0.,0.)) ;
#12668 = DIRECTION('center_axis',(-1.,0.,0.)) ;
#12669 = DIRECTION('ref_axis',(0.,0.,-1.)) ;
#12670 = DIRECTION('center_axis',(-1.,0.,0.)) ;
#12671 = DIRECTION('ref_axis',(0.,0.,1.)) ;
#12672 = DIRECTION('center_axis',(1.,0.,0.)) ;
#12673 = DIRECTION('ref_axis',(0.,0.,-1.)) ;
#12674 = DIRECTION('center_axis',(1.,0.,0.)) ;
#12675 = DIRECTION('ref_axis',(0.,0.,-1.)) ;
#12676 = DIRECTION('center_axis',(1.,0.,0.)) ;
#12677 = DIRECTION('ref_axis',(0.,0.,-1.)) ;
#12678 = DIRECTION('',(-1.,0.,0.)) ;
#12679 = DIRECTION('center_axis',(-1.,0.,0.)) ;
#12680 = DIRECTION('ref_axis',(0.,0.,-1.)) ;
#12681 = DIRECTION('center_axis',(-1.,0.,0.)) ;
#12682 = DIRECTION('ref_axis',(0.,0.,1.)) ;
#12683 = DIRECTION('center_axis',(1.,0.,0.)) ;
#12684 = DIRECTION('ref_axis',(0.,0.,-1.)) ;
#12685 = DIRECTION('axis',(0.,0.,1.)) ;
#12686 = DIRECTION('refdir',(1.,0.,0.)) ;
#12687 = DIRECTION('center_axis',(1.,0.,0.)) ;
#12688 = DIRECTION('ref_axis',(0.,0.,-1.)) ;
#12689 = DIRECTION('center_axis',(1.,0.,0.)) ;
#12690 = DIRECTION('ref_axis',(0.,0.,-1.)) ;
#12691 = DIRECTION('',(0.,1.,0.)) ;
#12692 = DIRECTION('',(0.,0.,-1.)) ;
#12693 = DIRECTION('',(0.,1.,0.)) ;
#12694 = DIRECTION('',(0.,0.,1.)) ;
#12695 = DIRECTION('',(0.,1.,0.)) ;
#12696 = DIRECTION('center_axis',(1.,0.,0.)) ;
#12697 = DIRECTION('ref_axis',(0.,0.,-1.)) ;
#12698 = DIRECTION('center_axis',(0.,0.,1.)) ;
#12699 = DIRECTION('ref_axis',(1.,0.,0.)) ;
#12700 = DIRECTION('',(1.,0.,0.)) ;
#12701 = DIRECTION('',(-1.,0.,0.)) ;
#12702 = DIRECTION('',(0.,-1.,0.)) ;
#12703 = DIRECTION('center_axis',(0.,0.,1.)) ;
#12704 = DIRECTION('ref_axis',(1.,0.,0.)) ;
#12705 = DIRECTION('',(-1.,0.,0.)) ;
#12706 = DIRECTION('',(0.,-1.,0.)) ;
#12707 = DIRECTION('',(1.,0.,0.)) ;
#12708 = DIRECTION('center_axis',(-1.,0.,0.)) ;
#12709 = DIRECTION('ref_axis',(0.,0.,1.)) ;
#12710 = DIRECTION('center_axis',(-1.,0.,0.)) ;
#12711 = DIRECTION('ref_axis',(0.,0.,-1.)) ;
#12712 = DIRECTION('',(0.,0.,-1.)) ;
#12713 = DIRECTION('',(0.,-1.,0.)) ;
#12714 = DIRECTION('',(0.,0.,1.)) ;
#12715 = DIRECTION('center_axis',(-1.,0.,0.)) ;
#12716 = DIRECTION('ref_axis',(0.,0.,-1.)) ;
#12717 = DIRECTION('center_axis',(0.,-1.,0.)) ;
#12718 = DIRECTION('ref_axis',(0.,0.,-1.)) ;
#12719 = DIRECTION('',(-1.,0.,0.)) ;
#12720 = DIRECTION('',(0.,0.,-1.)) ;
#12721 = DIRECTION('',(1.,0.,0.)) ;
#12722 = DIRECTION('',(0.,0.,-1.)) ;
#12723 = DIRECTION('',(-1.,0.,0.)) ;
#12724 = DIRECTION('center_axis',(0.,0.,1.)) ;
#12725 = DIRECTION('ref_axis',(1.,0.,0.)) ;
#12726 = DIRECTION('',(1.,0.,0.)) ;
#12727 = DIRECTION('',(0.,1.,0.)) ;
#12728 = DIRECTION('center_axis',(0.,0.,1.)) ;
#12729 = DIRECTION('ref_axis',(1.,0.,0.)) ;
#12730 = DIRECTION('',(0.,-1.,0.)) ;
#12731 = DIRECTION('',(1.,0.,0.)) ;
#12732 = DIRECTION('center_axis',(1.,0.,0.)) ;
#12733 = DIRECTION('ref_axis',(0.,0.,-1.)) ;
#12734 = DIRECTION('center_axis',(1.,0.,0.)) ;
#12735 = DIRECTION('ref_axis',(0.,0.,-1.)) ;
#12736 = DIRECTION('',(1.,0.,0.)) ;
#12737 = DIRECTION('',(1.,0.,0.)) ;
#12738 = DIRECTION('center_axis',(-1.,0.,0.)) ;
#12739 = DIRECTION('ref_axis',(0.,0.,-1.)) ;
#12740 = DIRECTION('center_axis',(0.,0.,1.)) ;
#12741 = DIRECTION('ref_axis',(1.,0.,0.)) ;
#12742 = DIRECTION('',(0.,-1.,0.)) ;
#12743 = DIRECTION('',(-1.,0.,0.)) ;
#12744 = DIRECTION('',(0.,1.,0.)) ;
#12745 = DIRECTION('center_axis',(0.,1.,0.)) ;
#12746 = DIRECTION('ref_axis',(0.,0.,1.)) ;
#12747 = DIRECTION('',(0.,0.,-1.)) ;
#12748 = DIRECTION('',(0.,0.,-1.)) ;
#12749 = DIRECTION('center_axis',(1.,0.,0.)) ;
#12750 = DIRECTION('ref_axis',(0.,0.,-1.)) ;
#12751 = DIRECTION('center_axis',(-1.,0.,0.)) ;
#12752 = DIRECTION('ref_axis',(0.,0.,1.)) ;
#12753 = DIRECTION('axis',(0.,0.,1.)) ;
#12754 = DIRECTION('refdir',(1.,0.,0.)) ;
#12755 = DIRECTION('center_axis',(1.,0.,0.)) ;
#12756 = DIRECTION('ref_axis',(0.,0.,-1.)) ;
#12757 = DIRECTION('center_axis',(1.,0.,0.)) ;
#12758 = DIRECTION('ref_axis',(0.,0.,-1.)) ;
#12759 = DIRECTION('',(-1.,0.,0.)) ;
#12760 = DIRECTION('center_axis',(-1.,0.,0.)) ;
#12761 = DIRECTION('ref_axis',(0.,0.,-1.)) ;
#12762 = DIRECTION('center_axis',(-1.,0.,0.)) ;
#12763 = DIRECTION('ref_axis',(0.,0.,1.)) ;
#12764 = DIRECTION('center_axis',(1.,0.,0.)) ;
#12765 = DIRECTION('ref_axis',(0.,0.,-1.)) ;
#12766 = DIRECTION('center_axis',(1.,0.,0.)) ;
#12767 = DIRECTION('ref_axis',(0.,0.,-1.)) ;
#12768 = DIRECTION('center_axis',(1.,0.,0.)) ;
#12769 = DIRECTION('ref_axis',(0.,0.,-1.)) ;
#12770 = DIRECTION('',(-1.,0.,0.)) ;
#12771 = DIRECTION('center_axis',(-1.,0.,0.)) ;
#12772 = DIRECTION('ref_axis',(0.,0.,-1.)) ;
#12773 = DIRECTION('center_axis',(-1.,0.,0.)) ;
#12774 = DIRECTION('ref_axis',(0.,0.,1.)) ;
#12775 = DIRECTION('center_axis',(1.,0.,0.)) ;
#12776 = DIRECTION('ref_axis',(0.,0.,-1.)) ;
#12777 = DIRECTION('center_axis',(1.,0.,0.)) ;
#12778 = DIRECTION('ref_axis',(0.,0.,-1.)) ;
#12779 = DIRECTION('center_axis',(1.,0.,0.)) ;
#12780 = DIRECTION('ref_axis',(0.,0.,-1.)) ;
#12781 = DIRECTION('',(-1.,0.,0.)) ;
#12782 = DIRECTION('center_axis',(-1.,0.,0.)) ;
#12783 = DIRECTION('ref_axis',(0.,0.,-1.)) ;
#12784 = DIRECTION('center_axis',(-1.,0.,0.)) ;
#12785 = DIRECTION('ref_axis',(0.,0.,1.)) ;
#12786 = DIRECTION('center_axis',(1.,0.,0.)) ;
#12787 = DIRECTION('ref_axis',(0.,0.,-1.)) ;
#12788 = DIRECTION('axis',(0.,0.,1.)) ;
#12789 = DIRECTION('refdir',(1.,0.,0.)) ;
#12790 = DIRECTION('center_axis',(1.,0.,0.)) ;
#12791 = DIRECTION('ref_axis',(0.,0.,-1.)) ;
#12792 = DIRECTION('center_axis',(1.,0.,0.)) ;
#12793 = DIRECTION('ref_axis',(0.,0.,-1.)) ;
#12794 = DIRECTION('',(-1.,0.,0.)) ;
#12795 = DIRECTION('center_axis',(-1.,0.,0.)) ;
#12796 = DIRECTION('ref_axis',(0.,0.,-1.)) ;
#12797 = DIRECTION('center_axis',(-1.,0.,0.)) ;
#12798 = DIRECTION('ref_axis',(0.,0.,1.)) ;
#12799 = DIRECTION('center_axis',(1.,0.,0.)) ;
#12800 = DIRECTION('ref_axis',(0.,0.,-1.)) ;
#12801 = DIRECTION('',(0.,0.,1.)) ;
#12802 = DIRECTION('',(1.,0.,0.)) ;
#12803 = DIRECTION('',(0.,0.,1.)) ;
#12804 = DIRECTION('',(1.,0.,0.)) ;
#12805 = DIRECTION('',(0.,0.,1.)) ;
#12806 = DIRECTION('',(1.,0.,0.)) ;
#12807 = DIRECTION('',(0.,0.,1.)) ;
#12808 = DIRECTION('',(1.,0.,0.)) ;
#12809 = DIRECTION('',(0.,0.,1.)) ;
#12810 = DIRECTION('',(1.,0.,0.)) ;
#12811 = DIRECTION('',(0.,0.,1.)) ;
#12812 = DIRECTION('',(1.,0.,0.)) ;
#12813 = DIRECTION('',(0.,0.,1.)) ;
#12814 = DIRECTION('',(1.,0.,0.)) ;
#12815 = DIRECTION('',(0.,0.,1.)) ;
#12816 = DIRECTION('',(1.,0.,0.)) ;
#12817 = DIRECTION('',(0.,0.,1.)) ;
#12818 = DIRECTION('',(1.,0.,0.)) ;
#12819 = DIRECTION('axis',(0.,0.,1.)) ;
#12820 = DIRECTION('refdir',(1.,0.,0.)) ;
#12821 = DIRECTION('axis',(0.,0.,1.)) ;
#12822 = DIRECTION('refdir',(1.,0.,0.)) ;
#12823 = DIRECTION('center_axis',(0.,0.,1.)) ;
#12824 = DIRECTION('ref_axis',(1.,0.,0.)) ;
#12825 = DIRECTION('center_axis',(0.,0.,1.)) ;
#12826 = DIRECTION('ref_axis',(1.,0.,0.)) ;
#12827 = DIRECTION('',(0.,0.,-1.)) ;
#12828 = DIRECTION('center_axis',(0.,0.,-1.)) ;
#12829 = DIRECTION('ref_axis',(1.,0.,0.)) ;
#12830 = DIRECTION('center_axis',(0.,0.,1.)) ;
#12831 = DIRECTION('ref_axis',(1.,0.,0.)) ;
#12832 = DIRECTION('center_axis',(0.,0.,1.)) ;
#12833 = DIRECTION('ref_axis',(1.,0.,0.)) ;
#12834 = DIRECTION('center_axis',(0.,0.,1.)) ;
#12835 = DIRECTION('ref_axis',(1.,0.,0.)) ;
#12836 = DIRECTION('',(0.,0.,-1.)) ;
#12837 = DIRECTION('center_axis',(0.,0.,-1.)) ;
#12838 = DIRECTION('ref_axis',(1.,0.,0.)) ;
#12839 = DIRECTION('center_axis',(0.,0.,-1.)) ;
#12840 = DIRECTION('ref_axis',(-1.,0.,0.)) ;
#12841 = DIRECTION('center_axis',(0.,0.,1.)) ;
#12842 = DIRECTION('ref_axis',(1.,0.,0.)) ;
#12843 = DIRECTION('axis',(0.,0.,1.)) ;
#12844 = DIRECTION('refdir',(1.,0.,0.)) ;
#12845 = DIRECTION('center_axis',(0.,0.,1.)) ;
#12846 = DIRECTION('ref_axis',(1.,0.,0.)) ;
#12847 = DIRECTION('center_axis',(0.,0.,1.)) ;
#12848 = DIRECTION('ref_axis',(1.,0.,0.)) ;
#12849 = DIRECTION('',(0.,0.,-1.)) ;
#12850 = DIRECTION('center_axis',(0.,0.,-1.)) ;
#12851 = DIRECTION('ref_axis',(1.,0.,0.)) ;
#12852 = DIRECTION('center_axis',(0.,0.,1.)) ;
#12853 = DIRECTION('ref_axis',(1.,0.,0.)) ;
#12854 = DIRECTION('center_axis',(0.,0.,1.)) ;
#12855 = DIRECTION('ref_axis',(1.,0.,0.)) ;
#12856 = DIRECTION('center_axis',(0.,0.,1.)) ;
#12857 = DIRECTION('ref_axis',(1.,0.,0.)) ;
#12858 = DIRECTION('',(0.,0.,-1.)) ;
#12859 = DIRECTION('center_axis',(0.,0.,-1.)) ;
#12860 = DIRECTION('ref_axis',(1.,0.,0.)) ;
#12861 = DIRECTION('center_axis',(0.,0.,-1.)) ;
#12862 = DIRECTION('ref_axis',(-1.,0.,0.)) ;
#12863 = DIRECTION('center_axis',(0.,0.,1.)) ;
#12864 = DIRECTION('ref_axis',(1.,0.,0.)) ;
#12865 = DIRECTION('',(0.,0.,1.)) ;
#12866 = DIRECTION('',(1.,0.,0.)) ;
#12867 = DIRECTION('',(0.,0.,1.)) ;
#12868 = DIRECTION('',(1.,0.,0.)) ;
#12869 = DIRECTION('',(0.,0.,1.)) ;
#12870 = DIRECTION('',(1.,0.,0.)) ;
#12871 = DIRECTION('',(0.,0.,1.)) ;
#12872 = DIRECTION('',(1.,0.,0.)) ;
#12873 = DIRECTION('',(0.,0.,1.)) ;
#12874 = DIRECTION('',(1.,0.,0.)) ;
#12875 = DIRECTION('',(0.,0.,1.)) ;
#12876 = DIRECTION('',(1.,0.,0.)) ;
#12877 = DIRECTION('',(0.,0.,1.)) ;
#12878 = DIRECTION('',(1.,0.,0.)) ;
#12879 = DIRECTION('',(0.,0.,1.)) ;
#12880 = DIRECTION('',(1.,0.,0.)) ;
#12881 = DIRECTION('',(0.,0.,1.)) ;
#12882 = DIRECTION('',(1.,0.,0.)) ;
#12883 = DIRECTION('',(0.,0.,1.)) ;
#12884 = DIRECTION('',(1.,0.,0.)) ;
#12885 = CARTESIAN_POINT('',(0.,0.,0.)) ;
#12886 = CARTESIAN_POINT('',(0.,0.,0.)) ;
#12887 = CARTESIAN_POINT('',(0.,0.,0.)) ;
#12888 = CARTESIAN_POINT('Origin',(-3.2,-2.15,0.2)) ;
#12889 = CARTESIAN_POINT('',(-2.7,-2.,0.2)) ;
#12890 = CARTESIAN_POINT('',(-2.7,-2.3,0.2)) ;
#12891 = CARTESIAN_POINT('',(-2.7,-2.15,0.2)) ;
#12892 = CARTESIAN_POINT('',(-3.7,-2.,0.2)) ;
#12893 = CARTESIAN_POINT('',(-3.2,-2.,0.2)) ;
#12894 = CARTESIAN_POINT('',(-3.7,-2.3,0.2)) ;
#12895 = CARTESIAN_POINT('',(-3.7,-1.075,0.2)) ;
#12896 = CARTESIAN_POINT('',(-1.6,-2.3,0.2)) ;
#12897 = CARTESIAN_POINT('Origin',(0.,-2.3,0.9)) ;
#12898 = CARTESIAN_POINT('',(-3.7,-2.3,1.4)) ;
#12899 = CARTESIAN_POINT('',(-3.7,-2.3,0.2)) ;
#12900 = CARTESIAN_POINT('',(3.7,-2.3,1.4)) ;
#12901 = CARTESIAN_POINT('',(0.,-2.3,1.4)) ;
#12902 = CARTESIAN_POINT('',(3.7,-2.3,0.3)) ;
#12903 = CARTESIAN_POINT('',(3.7,-2.3,0.9)) ;
#12904 = CARTESIAN_POINT('',(-2.7,-2.3,0.3)) ;
#12905 = CARTESIAN_POINT('',(0.,-2.3,0.3)) ;
#12906 = CARTESIAN_POINT('',(-2.7,-2.3,0.2)) ;
#12907 = CARTESIAN_POINT('Origin',(-3.7,0.,0.9)) ;
#12908 = CARTESIAN_POINT('',(-3.7,-2.,0.3)) ;
#12909 = CARTESIAN_POINT('',(-3.7,-2.,0.2)) ;
#12910 = CARTESIAN_POINT('',(-3.7,2.3,0.3)) ;
#12911 = CARTESIAN_POINT('',(-3.7,0.,0.3)) ;
#12912 = CARTESIAN_POINT('',(-3.7,2.3,1.4)) ;
#12913 = CARTESIAN_POINT('',(-3.7,2.3,0.9)) ;
#12914 = CARTESIAN_POINT('',(-3.7,0.,1.4)) ;
#12915 = CARTESIAN_POINT('Origin',(-3.2,-2.,0.2)) ;
#12916 = CARTESIAN_POINT('',(-2.7,-2.,0.3)) ;
#12917 = CARTESIAN_POINT('',(-2.7,-2.,0.2)) ;
#12918 = CARTESIAN_POINT('',(-1.6,-2.,0.3)) ;
#12919 = CARTESIAN_POINT('Origin',(-2.7,-2.15,0.2)) ;
#12920 = CARTESIAN_POINT('',(-2.7,-1.075,0.3)) ;
#12921 = CARTESIAN_POINT('Origin',(0.,0.,0.3)) ;
#12922 = CARTESIAN_POINT('',(3.7,2.3,0.3)) ;
#12923 = CARTESIAN_POINT('',(3.7,0.,0.3)) ;
#12924 = CARTESIAN_POINT('',(0.,2.3,0.3)) ;
#12925 = CARTESIAN_POINT('',(-0.4,-1.4,0.3)) ;
#12926 = CARTESIAN_POINT('Origin',(0.,-1.4,0.3)) ;
#12927 = CARTESIAN_POINT('',(-3.4,1.8,0.3)) ;
#12928 = CARTESIAN_POINT('Origin',(-3.,1.8,0.3)) ;
#12929 = CARTESIAN_POINT('',(0.8,0.9,0.3)) ;
#12930 = CARTESIAN_POINT('',(0.4,0.9,0.3)) ;
#12931 = CARTESIAN_POINT('',(0.3,0.9,0.3)) ;
#12932 = CARTESIAN_POINT('',(0.4,1.3,0.3)) ;
#12933 = CARTESIAN_POINT('',(0.4,0.55,0.3)) ;
#12934 = CARTESIAN_POINT('',(0.8,1.3,0.3)) ;
#12935 = CARTESIAN_POINT('',(0.3,1.3,0.3)) ;
#12936 = CARTESIAN_POINT('',(0.8,0.55,0.3)) ;
#12937 = CARTESIAN_POINT('',(0.8,0.1,0.3)) ;
#12938 = CARTESIAN_POINT('',(0.4,0.1,0.3)) ;
#12939 = CARTESIAN_POINT('',(0.3,0.1,0.3)) ;
#12940 = CARTESIAN_POINT('',(0.4,0.5,0.3)) ;
#12941 = CARTESIAN_POINT('',(0.4,0.15,0.3)) ;
#12942 = CARTESIAN_POINT('',(0.8,0.5,0.3)) ;
#12943 = CARTESIAN_POINT('',(0.3,0.5,0.3)) ;
#12944 = CARTESIAN_POINT('',(0.8,0.15,0.3)) ;
#12945 = CARTESIAN_POINT('',(-2.31,1.60428730688303E-16,0.3)) ;
#12946 = CARTESIAN_POINT('Origin',(-1.,0.,0.3)) ;
#12947 = CARTESIAN_POINT('',(1.,0.8,0.3)) ;
#12948 = CARTESIAN_POINT('Origin',(2.,0.8,0.3)) ;
#12949 = CARTESIAN_POINT('Origin',(3.6,-1.05,0.075)) ;
#12950 = CARTESIAN_POINT('',(3.445,-1.05,0.)) ;
#12951 = CARTESIAN_POINT('Origin',(3.6,-1.05,0.)) ;
#12952 = CARTESIAN_POINT('',(3.445,-1.05,0.25)) ;
#12953 = CARTESIAN_POINT('',(3.445,-1.05,0.075)) ;
#12954 = CARTESIAN_POINT('Origin',(3.6,-1.05,0.25)) ;
#12955 = CARTESIAN_POINT('Origin',(3.6,-1.05,0.25)) ;
#12956 = CARTESIAN_POINT('Origin',(2.8,-1.05,0.075)) ;
#12957 = CARTESIAN_POINT('',(2.645,-1.05,0.)) ;
#12958 = CARTESIAN_POINT('Origin',(2.8,-1.05,0.)) ;
#12959 = CARTESIAN_POINT('',(2.645,-1.05,0.25)) ;
#12960 = CARTESIAN_POINT('',(2.645,-1.05,0.075)) ;
#12961 = CARTESIAN_POINT('Origin',(2.8,-1.05,0.25)) ;
#12962 = CARTESIAN_POINT('Origin',(2.8,-1.05,0.25)) ;
#12963 = CARTESIAN_POINT('Origin',(0.,-2.85,0.15)) ;
#12964 = CARTESIAN_POINT('',(-0.17,-2.85,0.)) ;
#12965 = CARTESIAN_POINT('Origin',(0.,-2.85,0.)) ;
#12966 = CARTESIAN_POINT('',(-0.17,-2.85,0.3)) ;
#12967 = CARTESIAN_POINT('',(-0.17,-2.85,0.15)) ;
#12968 = CARTESIAN_POINT('Origin',(0.,-2.85,0.3)) ;
#12969 = CARTESIAN_POINT('Origin',(0.,-2.85,0.3)) ;
#12970 = CARTESIAN_POINT('',(0.8,-3.1,0.3)) ;
#12971 = CARTESIAN_POINT('',(0.8,-2.6,0.3)) ;
#12972 = CARTESIAN_POINT('',(0.8,-2.85,0.3)) ;
#12973 = CARTESIAN_POINT('',(-0.8,-2.6,0.3)) ;
#12974 = CARTESIAN_POINT('',(0.,-2.6,0.3)) ;
#12975 = CARTESIAN_POINT('',(-0.8,-3.1,0.3)) ;
#12976 = CARTESIAN_POINT('',(-0.8,-2.85,0.3)) ;
#12977 = CARTESIAN_POINT('',(0.,-3.1,0.3)) ;
#12978 = CARTESIAN_POINT('Origin',(0.,-3.1,0.15)) ;
#12979 = CARTESIAN_POINT('',(-0.8,-3.1,0.)) ;
#12980 = CARTESIAN_POINT('',(-0.8,-3.1,0.15)) ;
#12981 = CARTESIAN_POINT('',(0.8,-3.1,0.)) ;
#12982 = CARTESIAN_POINT('',(0.,-3.1,0.)) ;
#12983 = CARTESIAN_POINT('',(0.8,-3.1,0.15)) ;
#12984 = CARTESIAN_POINT('Origin',(-0.8,-2.85,0.15)) ;
#12985 = CARTESIAN_POINT('',(-0.8,-2.6,0.)) ;
#12986 = CARTESIAN_POINT('',(-0.8,-2.6,0.425)) ;
#12987 = CARTESIAN_POINT('',(-0.8,-2.85,0.)) ;
#12988 = CARTESIAN_POINT('Origin',(0.8,-2.85,0.15)) ;
#12989 = CARTESIAN_POINT('',(0.8,-2.6,0.)) ;
#12990 = CARTESIAN_POINT('',(0.8,-2.85,0.)) ;
#12991 = CARTESIAN_POINT('',(0.8,-2.6,0.425)) ;
#12992 = CARTESIAN_POINT('Origin',(0.,-2.6,0.7)) ;
#12993 = CARTESIAN_POINT('',(4.,-2.6,0.)) ;
#12994 = CARTESIAN_POINT('',(0.,-2.6,0.)) ;
#12995 = CARTESIAN_POINT('',(4.,-2.6,1.4)) ;
#12996 = CARTESIAN_POINT('',(4.,-2.6,0.7)) ;
#12997 = CARTESIAN_POINT('',(-4.,-2.6,1.4)) ;
#12998 = CARTESIAN_POINT('',(0.,-2.6,1.4)) ;
#12999 = CARTESIAN_POINT('',(-4.,-2.6,0.)) ;
#13000 = CARTESIAN_POINT('',(-4.,-2.6,0.7)) ;
#13001 = CARTESIAN_POINT('',(0.,-2.6,0.)) ;
#13002 = CARTESIAN_POINT('Origin',(0.,2.85,0.15)) ;
#13003 = CARTESIAN_POINT('',(-0.17,2.85,0.)) ;
#13004 = CARTESIAN_POINT('Origin',(0.,2.85,0.)) ;
#13005 = CARTESIAN_POINT('',(-0.17,2.85,0.3)) ;
#13006 = CARTESIAN_POINT('',(-0.17,2.85,0.15)) ;
#13007 = CARTESIAN_POINT('Origin',(0.,2.85,0.3)) ;
#13008 = CARTESIAN_POINT('Origin',(0.,2.85,0.3)) ;
#13009 = CARTESIAN_POINT('',(0.8,2.6,0.3)) ;
#13010 = CARTESIAN_POINT('',(0.8,3.1,0.3)) ;
#13011 = CARTESIAN_POINT('',(0.8,2.85,0.3)) ;
#13012 = CARTESIAN_POINT('',(-0.8,3.1,0.3)) ;
#13013 = CARTESIAN_POINT('',(0.,3.1,0.3)) ;
#13014 = CARTESIAN_POINT('',(-0.8,2.6,0.3)) ;
#13015 = CARTESIAN_POINT('',(-0.8,2.85,0.3)) ;
#13016 = CARTESIAN_POINT('',(0.,2.6,0.3)) ;
#13017 = CARTESIAN_POINT('Origin',(-0.8,2.85,0.15)) ;
#13018 = CARTESIAN_POINT('',(-0.8,3.1,0.)) ;
#13019 = CARTESIAN_POINT('',(-0.8,3.1,0.15)) ;
#13020 = CARTESIAN_POINT('',(-0.8,2.6,0.)) ;
#13021 = CARTESIAN_POINT('',(-0.8,2.85,0.)) ;
#13022 = CARTESIAN_POINT('',(-0.8,2.6,0.425)) ;
#13023 = CARTESIAN_POINT('Origin',(0.,3.1,0.15)) ;
#13024 = CARTESIAN_POINT('',(0.8,3.1,0.)) ;
#13025 = CARTESIAN_POINT('',(0.8,3.1,0.15)) ;
#13026 = CARTESIAN_POINT('',(0.,3.1,0.)) ;
#13027 = CARTESIAN_POINT('Origin',(0.8,2.85,0.15)) ;
#13028 = CARTESIAN_POINT('',(0.8,2.6,0.)) ;
#13029 = CARTESIAN_POINT('',(0.8,2.6,0.425)) ;
#13030 = CARTESIAN_POINT('',(0.8,2.85,0.)) ;
#13031 = CARTESIAN_POINT('Origin',(0.,2.6,0.7)) ;
#13032 = CARTESIAN_POINT('',(-4.,2.6,0.)) ;
#13033 = CARTESIAN_POINT('',(0.,2.6,0.)) ;
#13034 = CARTESIAN_POINT('',(-4.,2.6,1.4)) ;
#13035 = CARTESIAN_POINT('',(-4.,2.6,0.7)) ;
#13036 = CARTESIAN_POINT('',(4.,2.6,1.4)) ;
#13037 = CARTESIAN_POINT('',(0.,2.6,1.4)) ;
#13038 = CARTESIAN_POINT('',(4.,2.6,0.)) ;
#13039 = CARTESIAN_POINT('',(4.,2.6,0.7)) ;
#13040 = CARTESIAN_POINT('',(0.,2.6,0.)) ;
#13041 = CARTESIAN_POINT('Origin',(0.,-1.4,0.7)) ;
#13042 = CARTESIAN_POINT('',(-0.14,-1.4,0.3)) ;
#13043 = CARTESIAN_POINT('Origin',(0.,-1.4,0.3)) ;
#13044 = CARTESIAN_POINT('',(-0.14,-1.4,1.1)) ;
#13045 = CARTESIAN_POINT('',(-0.14,-1.4,0.7)) ;
#13046 = CARTESIAN_POINT('Origin',(0.,-1.4,1.1)) ;
#13047 = CARTESIAN_POINT('Origin',(0.,-1.4,0.7)) ;
#13048 = CARTESIAN_POINT('',(-0.4,-1.4,1.1)) ;
#13049 = CARTESIAN_POINT('Origin',(0.,-1.4,1.1)) ;
#13050 = CARTESIAN_POINT('',(-0.4,-1.4,0.7)) ;
#13051 = CARTESIAN_POINT('Origin',(0.,-1.4,1.1)) ;
#13052 = CARTESIAN_POINT('Origin',(0.,0.,0.3)) ;
#13053 = CARTESIAN_POINT('Origin',(2.,0.8,0.5)) ;
#13054 = CARTESIAN_POINT('',(1.2,0.8,0.3)) ;
#13055 = CARTESIAN_POINT('Origin',(2.,0.8,0.3)) ;
#13056 = CARTESIAN_POINT('',(1.2,0.8,0.7)) ;
#13057 = CARTESIAN_POINT('',(1.2,0.8,0.5)) ;
#13058 = CARTESIAN_POINT('Origin',(2.,0.8,0.7)) ;
#13059 = CARTESIAN_POINT('Origin',(2.,0.8,0.5)) ;
#13060 = CARTESIAN_POINT('',(1.,0.8,0.7)) ;
#13061 = CARTESIAN_POINT('Origin',(2.,0.8,0.7)) ;
#13062 = CARTESIAN_POINT('',(1.,0.8,0.5)) ;
#13063 = CARTESIAN_POINT('Origin',(2.,0.8,0.7)) ;
#13064 = CARTESIAN_POINT('Origin',(-3.,1.8,0.95)) ;
#13065 = CARTESIAN_POINT('',(-3.21,1.8,0.3)) ;
#13066 = CARTESIAN_POINT('Origin',(-3.,1.8,0.3)) ;
#13067 = CARTESIAN_POINT('',(-3.21,1.8,1.6)) ;
#13068 = CARTESIAN_POINT('',(-3.21,1.8,0.95)) ;
#13069 = CARTESIAN_POINT('Origin',(-3.,1.8,1.6)) ;
#13070 = CARTESIAN_POINT('Origin',(-3.,1.8,0.95)) ;
#13071 = CARTESIAN_POINT('',(-3.4,1.8,1.6)) ;
#13072 = CARTESIAN_POINT('Origin',(-3.,1.8,1.6)) ;
#13073 = CARTESIAN_POINT('',(-3.4,1.8,0.95)) ;
#13074 = CARTESIAN_POINT('Origin',(-3.,1.8,1.6)) ;
#13075 = CARTESIAN_POINT('Origin',(0.,0.,0.3)) ;
#13076 = CARTESIAN_POINT('Origin',(0.6,0.7,2.3)) ;
#13077 = CARTESIAN_POINT('',(0.47,0.1,2.3)) ;
#13078 = CARTESIAN_POINT('Origin',(0.6,0.1,2.3)) ;
#13079 = CARTESIAN_POINT('',(0.47,0.5,2.3)) ;
#13080 = CARTESIAN_POINT('',(0.47,0.7,2.3)) ;
#13081 = CARTESIAN_POINT('Origin',(0.6,0.5,2.3)) ;
#13082 = CARTESIAN_POINT('Origin',(0.6,0.7,2.3)) ;
#13083 = CARTESIAN_POINT('',(0.47,0.9,2.3)) ;
#13084 = CARTESIAN_POINT('Origin',(0.6,0.9,2.3)) ;
#13085 = CARTESIAN_POINT('',(0.47,1.3,2.3)) ;
#13086 = CARTESIAN_POINT('',(0.47,0.7,2.3)) ;
#13087 = CARTESIAN_POINT('Origin',(0.6,1.3,2.3)) ;
#13088 = CARTESIAN_POINT('Origin',(0.6,1.1,2.7)) ;
#13089 = CARTESIAN_POINT('',(0.8,0.9,2.7)) ;
#13090 = CARTESIAN_POINT('',(0.8,1.3,2.7)) ;
#13091 = CARTESIAN_POINT('',(0.8,1.1,2.7)) ;
#13092 = CARTESIAN_POINT('',(0.4,1.3,2.7)) ;
#13093 = CARTESIAN_POINT('',(0.6,1.3,2.7)) ;
#13094 = CARTESIAN_POINT('',(0.4,0.9,2.7)) ;
#13095 = CARTESIAN_POINT('',(0.4,1.1,2.7)) ;
#13096 = CARTESIAN_POINT('',(0.6,0.9,2.7)) ;
#13097 = CARTESIAN_POINT('Origin',(0.6,0.9,1.5)) ;
#13098 = CARTESIAN_POINT('',(0.4,0.9,1.5)) ;
#13099 = CARTESIAN_POINT('',(0.8,0.9,1.5)) ;
#13100 = CARTESIAN_POINT('Origin',(0.4,1.1,1.5)) ;
#13101 = CARTESIAN_POINT('',(0.4,1.3,1.5)) ;
#13102 = CARTESIAN_POINT('Origin',(0.6,1.3,1.5)) ;
#13103 = CARTESIAN_POINT('',(0.8,1.3,1.5)) ;
#13104 = CARTESIAN_POINT('Origin',(0.8,1.1,1.5)) ;
#13105 = CARTESIAN_POINT('Origin',(0.6,0.3,2.7)) ;
#13106 = CARTESIAN_POINT('',(0.8,0.1,2.7)) ;
#13107 = CARTESIAN_POINT('',(0.8,0.5,2.7)) ;
#13108 = CARTESIAN_POINT('',(0.8,0.3,2.7)) ;
#13109 = CARTESIAN_POINT('',(0.4,0.5,2.7)) ;
#13110 = CARTESIAN_POINT('',(0.6,0.5,2.7)) ;
#13111 = CARTESIAN_POINT('',(0.4,0.1,2.7)) ;
#13112 = CARTESIAN_POINT('',(0.4,0.3,2.7)) ;
#13113 = CARTESIAN_POINT('',(0.6,0.1,2.7)) ;
#13114 = CARTESIAN_POINT('Origin',(0.6,0.1,1.5)) ;
#13115 = CARTESIAN_POINT('',(0.4,0.1,1.5)) ;
#13116 = CARTESIAN_POINT('',(0.8,0.1,1.5)) ;
#13117 = CARTESIAN_POINT('Origin',(0.4,0.3,1.5)) ;
#13118 = CARTESIAN_POINT('',(0.4,0.5,1.5)) ;
#13119 = CARTESIAN_POINT('Origin',(0.6,0.5,1.5)) ;
#13120 = CARTESIAN_POINT('',(0.8,0.5,1.5)) ;
#13121 = CARTESIAN_POINT('Origin',(0.8,0.3,1.5)) ;
#13122 = CARTESIAN_POINT('Origin',(-1.,0.,0.15)) ;
#13123 = CARTESIAN_POINT('',(-2.31,-1.60428730688303E-16,0.)) ;
#13124 = CARTESIAN_POINT('Origin',(-1.,0.,0.)) ;
#13125 = CARTESIAN_POINT('',(-2.31,-1.60428730688303E-16,0.15)) ;
#13126 = CARTESIAN_POINT('Origin',(0.,2.3,0.9)) ;
#13127 = CARTESIAN_POINT('',(3.7,2.3,1.4)) ;
#13128 = CARTESIAN_POINT('',(0.,2.3,1.4)) ;
#13129 = CARTESIAN_POINT('',(3.7,2.3,0.9)) ;
#13130 = CARTESIAN_POINT('Origin',(3.7,0.,0.9)) ;
#13131 = CARTESIAN_POINT('',(3.7,0.,1.4)) ;
#13132 = CARTESIAN_POINT('Origin',(0.,0.,0.3)) ;
#13133 = CARTESIAN_POINT('Origin',(0.,0.,1.4)) ;
#13134 = CARTESIAN_POINT('',(4.,0.,1.4)) ;
#13135 = CARTESIAN_POINT('',(-4.,0.,1.4)) ;
#13136 = CARTESIAN_POINT('Origin',(0.,0.,0.)) ;
#13137 = CARTESIAN_POINT('',(4.,0.,0.)) ;
#13138 = CARTESIAN_POINT('',(-4.,0.,0.)) ;
#13139 = CARTESIAN_POINT('Origin',(-4.,0.,0.7)) ;
#13140 = CARTESIAN_POINT('Origin',(4.,0.,0.7)) ;
#13141 = CARTESIAN_POINT('',(0.,0.,0.)) ;
#13142 = CARTESIAN_POINT('Origin',(3.6,-1.05,-0.745)) ;
#13143 = CARTESIAN_POINT('',(3.8,-0.833147515577986,-0.59)) ;
#13144 = CARTESIAN_POINT('',(3.8,-0.833147515577986,-0.8)) ;
#13145 = CARTESIAN_POINT('',(3.8,-0.833147515577986,-0.745)) ;
#13146 = CARTESIAN_POINT('',(3.75660459763366,-0.8,-0.59)) ;
#13147 = CARTESIAN_POINT('Origin',(3.6,-1.05,-0.59)) ;
#13148 = CARTESIAN_POINT('',(3.75660459763366,-0.8,-0.8)) ;
#13149 = CARTESIAN_POINT('',(3.75660459763366,-0.8,-0.745)) ;
#13150 = CARTESIAN_POINT('Origin',(3.6,-1.05,-0.8)) ;
#13151 = CARTESIAN_POINT('Origin',(3.6,-1.05,-0.59)) ;
#13152 = CARTESIAN_POINT('',(3.8,-1.26685248442201,-0.59)) ;
#13153 = CARTESIAN_POINT('',(3.8,-1.275,-0.59)) ;
#13154 = CARTESIAN_POINT('',(3.44339540236634,-0.8,-0.59)) ;
#13155 = CARTESIAN_POINT('Origin',(3.6,-1.05,-0.59)) ;
#13156 = CARTESIAN_POINT('',(3.4,-0.8,-0.59)) ;
#13157 = CARTESIAN_POINT('',(3.43,-1.05,-0.59)) ;
#13158 = CARTESIAN_POINT('Origin',(3.6,-1.05,-0.59)) ;
#13159 = CARTESIAN_POINT('Origin',(3.6,-1.05,-0.745)) ;
#13160 = CARTESIAN_POINT('',(3.8,-1.26685248442201,-0.8)) ;
#13161 = CARTESIAN_POINT('',(3.8,-1.26685248442201,-0.745)) ;
#13162 = CARTESIAN_POINT('',(3.44339540236634,-0.8,-0.8)) ;
#13163 = CARTESIAN_POINT('Origin',(3.6,-1.05,-0.8)) ;
#13164 = CARTESIAN_POINT('',(3.44339540236634,-0.8,-0.745)) ;
#13165 = CARTESIAN_POINT('Origin',(3.8,-1.5,-0.4)) ;
#13166 = CARTESIAN_POINT('',(3.8,-0.8,-0.8)) ;
#13167 = CARTESIAN_POINT('',(3.8,-1.5,-0.8)) ;
#13168 = CARTESIAN_POINT('',(3.8,-0.8,0.)) ;
#13169 = CARTESIAN_POINT('',(3.8,-0.8,-0.4)) ;
#13170 = CARTESIAN_POINT('',(3.8,-2.2,0.)) ;
#13171 = CARTESIAN_POINT('',(3.8,-1.5,0.)) ;
#13172 = CARTESIAN_POINT('',(3.8,-2.2,-0.8)) ;
#13173 = CARTESIAN_POINT('',(3.8,-2.2,-0.4)) ;
#13174 = CARTESIAN_POINT('',(3.8,-1.5,-0.8)) ;
#13175 = CARTESIAN_POINT('',(3.8,-1.6,-0.09)) ;
#13176 = CARTESIAN_POINT('Origin',(3.8,-1.6,-0.4)) ;
#13177 = CARTESIAN_POINT('Origin',(3.2,-1.5,-0.8)) ;
#13178 = CARTESIAN_POINT('',(3.2,-0.8,-0.8)) ;
#13179 = CARTESIAN_POINT('Origin',(3.6,-1.05,-0.4)) ;
#13180 = CARTESIAN_POINT('',(3.43,-1.05,0.)) ;
#13181 = CARTESIAN_POINT('',(3.43,-1.05,-0.4)) ;
#13182 = CARTESIAN_POINT('Origin',(3.6,-1.05,0.)) ;
#13183 = CARTESIAN_POINT('Origin',(2.8,-1.05,-0.745)) ;
#13184 = CARTESIAN_POINT('',(2.6,-0.833147515577986,-0.8)) ;
#13185 = CARTESIAN_POINT('',(2.6,-0.833147515577986,-0.59)) ;
#13186 = CARTESIAN_POINT('',(2.6,-0.833147515577986,-0.745)) ;
#13187 = CARTESIAN_POINT('',(2.64339540236634,-0.8,-0.8)) ;
#13188 = CARTESIAN_POINT('Origin',(2.8,-1.05,-0.8)) ;
#13189 = CARTESIAN_POINT('',(2.64339540236634,-0.8,-0.59)) ;
#13190 = CARTESIAN_POINT('',(2.64339540236634,-0.8,-0.745)) ;
#13191 = CARTESIAN_POINT('Origin',(2.8,-1.05,-0.59)) ;
#13192 = CARTESIAN_POINT('Origin',(2.8,-1.05,-0.745)) ;
#13193 = CARTESIAN_POINT('',(2.6,-1.26685248442201,-0.59)) ;
#13194 = CARTESIAN_POINT('',(2.6,-1.26685248442201,-0.8)) ;
#13195 = CARTESIAN_POINT('',(2.6,-1.26685248442201,-0.745)) ;
#13196 = CARTESIAN_POINT('',(2.95660459763366,-0.8,-0.59)) ;
#13197 = CARTESIAN_POINT('Origin',(2.8,-1.05,-0.59)) ;
#13198 = CARTESIAN_POINT('',(2.95660459763366,-0.8,-0.8)) ;
#13199 = CARTESIAN_POINT('',(2.95660459763366,-0.8,-0.745)) ;
#13200 = CARTESIAN_POINT('Origin',(2.8,-1.05,-0.8)) ;
#13201 = CARTESIAN_POINT('Origin',(2.8,-1.05,-0.59)) ;
#13202 = CARTESIAN_POINT('',(2.6,-1.275,-0.59)) ;
#13203 = CARTESIAN_POINT('',(3.,-0.8,-0.59)) ;
#13204 = CARTESIAN_POINT('',(2.63,-1.05,-0.59)) ;
#13205 = CARTESIAN_POINT('Origin',(2.8,-1.05,-0.59)) ;
#13206 = CARTESIAN_POINT('Origin',(3.2,-0.8,-0.4)) ;
#13207 = CARTESIAN_POINT('',(3.2,-0.8,-0.8)) ;
#13208 = CARTESIAN_POINT('',(2.6,-0.8,-0.8)) ;
#13209 = CARTESIAN_POINT('',(3.2,-0.8,-0.8)) ;
#13210 = CARTESIAN_POINT('',(2.6,-0.8,0.)) ;
#13211 = CARTESIAN_POINT('',(2.6,-0.8,-0.4)) ;
#13212 = CARTESIAN_POINT('',(3.2,-0.8,0.)) ;
#13213 = CARTESIAN_POINT('Origin',(3.2,-1.5,-0.8)) ;
#13214 = CARTESIAN_POINT('',(2.6,-1.5,-0.8)) ;
#13215 = CARTESIAN_POINT('Origin',(3.2,-1.5,-0.8)) ;
#13216 = CARTESIAN_POINT('',(2.6,-2.2,-0.8)) ;
#13217 = CARTESIAN_POINT('',(3.2,-2.2,-0.8)) ;
#13218 = CARTESIAN_POINT('',(2.6,-1.5,-0.8)) ;
#13219 = CARTESIAN_POINT('Origin',(2.8,-1.05,-0.4)) ;
#13220 = CARTESIAN_POINT('',(2.63,-1.05,0.)) ;
#13221 = CARTESIAN_POINT('',(2.63,-1.05,-0.4)) ;
#13222 = CARTESIAN_POINT('Origin',(2.8,-1.05,0.)) ;
#13223 = CARTESIAN_POINT('Origin',(3.2,-1.6,-0.4)) ;
#13224 = CARTESIAN_POINT('',(2.6,-1.6,-0.09)) ;
#13225 = CARTESIAN_POINT('Origin',(2.6,-1.6,-0.4)) ;
#13226 = CARTESIAN_POINT('',(3.2,-1.6,-0.09)) ;
#13227 = CARTESIAN_POINT('Origin',(3.2,-1.5,0.)) ;
#13228 = CARTESIAN_POINT('',(2.6,-2.2,0.)) ;
#13229 = CARTESIAN_POINT('',(2.6,-1.5,0.)) ;
#13230 = CARTESIAN_POINT('',(3.2,-2.2,0.)) ;
#13231 = CARTESIAN_POINT('Origin',(3.2,-2.2,-0.4)) ;
#13232 = CARTESIAN_POINT('',(2.6,-2.2,-0.4)) ;
#13233 = CARTESIAN_POINT('Origin',(2.6,-1.5,-0.4)) ;
#13234 = CARTESIAN_POINT('',(0.,0.,0.)) ;
#13235 = CARTESIAN_POINT('',(0.,0.,0.)) ;
#13236 = CARTESIAN_POINT('',(0.,0.,0.)) ;
#13237 = CARTESIAN_POINT('',(0.,0.,0.)) ;
#13238 = CARTESIAN_POINT('Origin',(-1.,0.,-0.74)) ;
#13239 = CARTESIAN_POINT('',(-1.26,-3.18408167778312E-17,-1.2)) ;
#13240 = CARTESIAN_POINT('Origin',(-1.,0.,-1.2)) ;
#13241 = CARTESIAN_POINT('',(-1.26,-3.18408167778312E-17,-0.18)) ;
#13242 = CARTESIAN_POINT('',(-1.26,-3.18408167778312E-17,-0.74)) ;
#13243 = CARTESIAN_POINT('Origin',(-1.,0.,-0.18)) ;
#13244 = CARTESIAN_POINT('Origin',(-1.,0.,-0.18)) ;
#13245 = CARTESIAN_POINT('Origin',(-1.,-0.7,0.4)) ;
#13246 = CARTESIAN_POINT('',(-1.2,-0.7,0.5)) ;
#13247 = CARTESIAN_POINT('',(-0.8,-0.7,0.5)) ;
#13248 = CARTESIAN_POINT('',(-1.,-0.7,0.5)) ;
#13249 = CARTESIAN_POINT('',(-1.2,-0.7,0.2)) ;
#13250 = CARTESIAN_POINT('',(-1.2,-0.7,0.4)) ;
#13251 = CARTESIAN_POINT('',(-0.8,-0.7,0.2)) ;
#13252 = CARTESIAN_POINT('',(-1.,-0.7,0.2)) ;
#13253 = CARTESIAN_POINT('',(-0.8,-0.7,0.4)) ;
#13254 = CARTESIAN_POINT('Origin',(-0.8,-0.9,0.4)) ;
#13255 = CARTESIAN_POINT('',(-0.8,-1.1,0.5)) ;
#13256 = CARTESIAN_POINT('',(-0.8,-0.45,0.5)) ;
#13257 = CARTESIAN_POINT('',(-0.8,-1.1,0.2)) ;
#13258 = CARTESIAN_POINT('',(-0.8,-0.9,0.2)) ;
#13259 = CARTESIAN_POINT('',(-0.8,-1.1,0.4)) ;
#13260 = CARTESIAN_POINT('Origin',(-1.,-0.9,0.2)) ;
#13261 = CARTESIAN_POINT('',(-1.2,-1.1,0.2)) ;
#13262 = CARTESIAN_POINT('',(-1.2,-0.9,0.2)) ;
#13263 = CARTESIAN_POINT('',(-1.,-1.1,0.2)) ;
#13264 = CARTESIAN_POINT('Origin',(-1.,-1.1,0.4)) ;
#13265 = CARTESIAN_POINT('',(-1.2,-1.1,0.5)) ;
#13266 = CARTESIAN_POINT('',(-1.,-1.1,0.5)) ;
#13267 = CARTESIAN_POINT('',(-1.2,-1.1,0.4)) ;
#13268 = CARTESIAN_POINT('Origin',(-1.2,-0.9,0.4)) ;
#13269 = CARTESIAN_POINT('',(-1.2,-0.45,0.5)) ;
#13270 = CARTESIAN_POINT('Origin',(-1.77942286340599,0.65,0.4)) ;
#13271 = CARTESIAN_POINT('',(-1.97942286340599,0.65,0.5)) ;
#13272 = CARTESIAN_POINT('',(-1.579422863406,0.65,0.5)) ;
#13273 = CARTESIAN_POINT('',(-1.389711431703,0.65,0.5)) ;
#13274 = CARTESIAN_POINT('',(-1.97942286340599,0.65,0.2)) ;
#13275 = CARTESIAN_POINT('',(-1.97942286340599,0.65,0.4)) ;
#13276 = CARTESIAN_POINT('',(-1.579422863406,0.65,0.2)) ;
#13277 = CARTESIAN_POINT('',(-1.77942286340599,0.65,0.2)) ;
#13278 = CARTESIAN_POINT('',(-1.579422863406,0.65,0.4)) ;
#13279 = CARTESIAN_POINT('Origin',(-1.579422863406,0.45,0.4)) ;
#13280 = CARTESIAN_POINT('',(-1.579422863406,0.25,0.5)) ;
#13281 = CARTESIAN_POINT('',(-1.57942286340599,0.225,0.5)) ;
#13282 = CARTESIAN_POINT('',(-1.579422863406,0.25,0.2)) ;
#13283 = CARTESIAN_POINT('',(-1.579422863406,0.45,0.2)) ;
#13284 = CARTESIAN_POINT('',(-1.579422863406,0.25,0.4)) ;
#13285 = CARTESIAN_POINT('Origin',(-1.77942286340599,0.45,0.2)) ;
#13286 = CARTESIAN_POINT('',(-1.97942286340599,0.25,0.2)) ;
#13287 = CARTESIAN_POINT('',(-1.97942286340599,0.45,0.2)) ;
#13288 = CARTESIAN_POINT('',(-1.77942286340599,0.25,0.2)) ;
#13289 = CARTESIAN_POINT('Origin',(-1.77942286340599,0.25,0.4)) ;
#13290 = CARTESIAN_POINT('',(-1.97942286340599,0.25,0.5)) ;
#13291 = CARTESIAN_POINT('',(-1.389711431703,0.25,0.5)) ;
#13292 = CARTESIAN_POINT('',(-1.97942286340599,0.25,0.4)) ;
#13293 = CARTESIAN_POINT('Origin',(-1.97942286340599,0.45,0.4)) ;
#13294 = CARTESIAN_POINT('',(-1.979422863406,0.225,0.5)) ;
#13295 = CARTESIAN_POINT('Origin',(-0.220577136594005,0.65,0.4)) ;
#13296 = CARTESIAN_POINT('',(-0.420577136594005,0.65,0.5)) ;
#13297 = CARTESIAN_POINT('',(-0.0205771365940052,0.65,0.5)) ;
#13298 = CARTESIAN_POINT('',(-0.610288568297003,0.65,0.5)) ;
#13299 = CARTESIAN_POINT('',(-0.420577136594005,0.65,0.2)) ;
#13300 = CARTESIAN_POINT('',(-0.420577136594005,0.65,0.4)) ;
#13301 = CARTESIAN_POINT('',(-0.0205771365940052,0.65,0.2)) ;
#13302 = CARTESIAN_POINT('',(-0.220577136594005,0.65,0.2)) ;
#13303 = CARTESIAN_POINT('',(-0.0205771365940052,0.65,0.4)) ;
#13304 = CARTESIAN_POINT('Origin',(-0.0205771365940052,0.45,0.4)) ;
#13305 = CARTESIAN_POINT('',(-0.0205771365940052,0.25,0.5)) ;
#13306 = CARTESIAN_POINT('',(-0.0205771365940052,0.225,0.5)) ;
#13307 = CARTESIAN_POINT('',(-0.0205771365940052,0.25,0.2)) ;
#13308 = CARTESIAN_POINT('',(-0.0205771365940052,0.45,0.2)) ;
#13309 = CARTESIAN_POINT('',(-0.0205771365940052,0.25,0.4)) ;
#13310 = CARTESIAN_POINT('Origin',(-0.220577136594005,0.45,0.2)) ;
#13311 = CARTESIAN_POINT('',(-0.420577136594005,0.25,0.2)) ;
#13312 = CARTESIAN_POINT('',(-0.420577136594005,0.45,0.2)) ;
#13313 = CARTESIAN_POINT('',(-0.220577136594005,0.25,0.2)) ;
#13314 = CARTESIAN_POINT('Origin',(-0.220577136594005,0.25,0.4)) ;
#13315 = CARTESIAN_POINT('',(-0.420577136594005,0.25,0.5)) ;
#13316 = CARTESIAN_POINT('',(-0.610288568297003,0.25,0.5)) ;
#13317 = CARTESIAN_POINT('',(-0.420577136594005,0.25,0.4)) ;
#13318 = CARTESIAN_POINT('Origin',(-0.420577136594005,0.45,0.4)) ;
#13319 = CARTESIAN_POINT('',(-0.420577136594005,0.225,0.5)) ;
#13320 = CARTESIAN_POINT('Origin',(-1.,0.,-0.79)) ;
#13321 = CARTESIAN_POINT('',(-1.69,8.45006291411674E-17,-0.28)) ;
#13322 = CARTESIAN_POINT('Origin',(-1.,0.,-0.28)) ;
#13323 = CARTESIAN_POINT('',(-1.69,8.45006291411674E-17,-1.2)) ;
#13324 = CARTESIAN_POINT('',(-1.69,-8.45006291411674E-17,-0.79)) ;
#13325 = CARTESIAN_POINT('Origin',(-1.,0.,-1.2)) ;
#13326 = CARTESIAN_POINT('Origin',(-1.,0.,-0.79)) ;
#13327 = CARTESIAN_POINT('',(-1.81,-9.91963907309356E-17,-1.2)) ;
#13328 = CARTESIAN_POINT('Origin',(-1.,0.,-1.2)) ;
#13329 = CARTESIAN_POINT('',(-1.81,-9.91963907309356E-17,-0.28)) ;
#13330 = CARTESIAN_POINT('',(-1.81,-9.91963907309356E-17,-0.79)) ;
#13331 = CARTESIAN_POINT('Origin',(-1.,0.,-0.28)) ;
#13332 = CARTESIAN_POINT('Origin',(-1.,0.,-0.28)) ;
#13333 = CARTESIAN_POINT('Origin',(-1.,0.,-1.2)) ;
#13334 = CARTESIAN_POINT('',(-2.09,1.33486501107061E-16,-1.2)) ;
#13335 = CARTESIAN_POINT('Origin',(-1.,0.,-1.2)) ;
#13336 = CARTESIAN_POINT('Origin',(-1.,0.,-0.79)) ;
#13337 = CARTESIAN_POINT('',(-2.09,1.33486501107061E-16,-0.28)) ;
#13338 = CARTESIAN_POINT('Origin',(-1.,0.,-0.28)) ;
#13339 = CARTESIAN_POINT('',(-2.09,-1.33486501107061E-16,-0.79)) ;
#13340 = CARTESIAN_POINT('Origin',(-1.,0.,-0.79)) ;
#13341 = CARTESIAN_POINT('',(-2.21,-1.4818226269683E-16,-1.2)) ;
#13342 = CARTESIAN_POINT('Origin',(-1.,0.,-1.2)) ;
#13343 = CARTESIAN_POINT('',(-2.21,-1.4818226269683E-16,-0.28)) ;
#13344 = CARTESIAN_POINT('',(-2.21,-1.4818226269683E-16,-0.79)) ;
#13345 = CARTESIAN_POINT('Origin',(-1.,0.,-0.28)) ;
#13346 = CARTESIAN_POINT('Origin',(-1.,0.,-0.28)) ;
#13347 = CARTESIAN_POINT('Origin',(-1.,0.,-1.2)) ;
#13348 = CARTESIAN_POINT('',(-2.3,-1.59204083889156E-16,-1.2)) ;
#13349 = CARTESIAN_POINT('Origin',(-1.,0.,-1.2)) ;
#13350 = CARTESIAN_POINT('Origin',(-1.,0.,-0.35)) ;
#13351 = CARTESIAN_POINT('',(-2.3,-1.59204083889156E-16,0.5)) ;
#13352 = CARTESIAN_POINT('Origin',(-1.,0.,0.5)) ;
#13353 = CARTESIAN_POINT('',(-2.3,-1.59204083889156E-16,-0.35)) ;
#13354 = CARTESIAN_POINT('Origin',(-1.,0.,-1.2)) ;
#13355 = CARTESIAN_POINT('Origin',(-1.,0.,0.5)) ;
#13356 = CARTESIAN_POINT('',(0.,0.,0.)) ;
#13357 = CARTESIAN_POINT('Origin',(-1.,0.,-0.7)) ;
#13358 = CARTESIAN_POINT('',(-2.1,-1.34711147906209E-16,-1.1)) ;
#13359 = CARTESIAN_POINT('Origin',(-1.,0.,-1.1)) ;
#13360 = CARTESIAN_POINT('',(-2.1,1.34711147906209E-16,-0.3)) ;
#13361 = CARTESIAN_POINT('',(-2.1,-1.34711147906209E-16,-0.7)) ;
#13362 = CARTESIAN_POINT('Origin',(-1.,0.,-0.3)) ;
#13363 = CARTESIAN_POINT('Origin',(-1.,0.,-0.7)) ;
#13364 = CARTESIAN_POINT('',(-2.2,-1.46957615897682E-16,-0.3)) ;
#13365 = CARTESIAN_POINT('Origin',(-1.,0.,-0.3)) ;
#13366 = CARTESIAN_POINT('',(-2.2,-1.46957615897682E-16,-1.1)) ;
#13367 = CARTESIAN_POINT('',(-2.2,-1.46957615897682E-16,-0.7)) ;
#13368 = CARTESIAN_POINT('Origin',(-1.,0.,-1.1)) ;
#13369 = CARTESIAN_POINT('Origin',(-1.,0.,-1.1)) ;
#13370 = CARTESIAN_POINT('Origin',(-1.,0.,-0.3)) ;
#13371 = CARTESIAN_POINT('',(0.,0.,0.)) ;
#13372 = CARTESIAN_POINT('Origin',(-1.,0.,-0.7)) ;
#13373 = CARTESIAN_POINT('',(-1.7,-8.57252759403147E-17,-1.1)) ;
#13374 = CARTESIAN_POINT('Origin',(-1.,0.,-1.1)) ;
#13375 = CARTESIAN_POINT('',(-1.7,8.57252759403147E-17,-0.3)) ;
#13376 = CARTESIAN_POINT('',(-1.7,-8.57252759403147E-17,-0.7)) ;
#13377 = CARTESIAN_POINT('Origin',(-1.,0.,-0.3)) ;
#13378 = CARTESIAN_POINT('Origin',(-1.,0.,-0.7)) ;
#13379 = CARTESIAN_POINT('',(-1.8,-9.79717439317883E-17,-0.3)) ;
#13380 = CARTESIAN_POINT('Origin',(-1.,0.,-0.3)) ;
#13381 = CARTESIAN_POINT('',(-1.8,-9.79717439317883E-17,-1.1)) ;
#13382 = CARTESIAN_POINT('',(-1.8,-9.79717439317883E-17,-0.7)) ;
#13383 = CARTESIAN_POINT('Origin',(-1.,0.,-1.1)) ;
#13384 = CARTESIAN_POINT('Origin',(-1.,0.,-1.1)) ;
#13385 = CARTESIAN_POINT('Origin',(-1.,0.,-0.3)) ;
#13386 = CARTESIAN_POINT('',(0.,0.,0.)) ;
#13387 = CARTESIAN_POINT('Origin',(-1.,0.,-1.1)) ;
#13388 = CARTESIAN_POINT('',(-1.25,-3.06161699786838E-17,-1.1)) ;
#13389 = CARTESIAN_POINT('Origin',(-1.,0.,-1.1)) ;
#13390 = CARTESIAN_POINT('',(-1.,-1.87469972832732E-33,-1.35)) ;
#13391 = CARTESIAN_POINT('Origin',(-1.,0.,-1.1)) ;
#13392 = CARTESIAN_POINT('Origin',(-1.,0.,-0.65)) ;
#13393 = CARTESIAN_POINT('',(-1.25,-3.06161699786838E-17,-0.2)) ;
#13394 = CARTESIAN_POINT('Origin',(-1.,0.,-0.2)) ;
#13395 = CARTESIAN_POINT('',(-1.25,-3.06161699786838E-17,-0.65)) ;
#13396 = CARTESIAN_POINT('Origin',(-1.,0.,-0.2)) ;
#13397 = CARTESIAN_POINT('',(0.,0.,0.)) ;
#13398 = CARTESIAN_POINT('',(0.,0.,0.)) ;
#13399 = CARTESIAN_POINT('',(0.,0.,0.)) ;
#13400 = CARTESIAN_POINT('',(0.,0.,0.)) ;
#13401 = CARTESIAN_POINT('',(0.,0.,0.)) ;
#13402 = CARTESIAN_POINT('',(0.,0.,0.)) ;
#13403 = CARTESIAN_POINT('Origin',(2.,0.8,0.75)) ;
#13404 = CARTESIAN_POINT('',(1.87,0.8,0.7)) ;
#13405 = CARTESIAN_POINT('Origin',(2.,0.8,0.7)) ;
#13406 = CARTESIAN_POINT('',(1.87,0.8,0.8)) ;
#13407 = CARTESIAN_POINT('',(1.87,0.8,0.75)) ;
#13408 = CARTESIAN_POINT('Origin',(2.,0.8,0.8)) ;
#13409 = CARTESIAN_POINT('Origin',(2.,0.8,1.)) ;
#13410 = CARTESIAN_POINT('',(1.3,0.8,0.8)) ;
#13411 = CARTESIAN_POINT('Origin',(2.,0.8,0.8)) ;
#13412 = CARTESIAN_POINT('',(1.3,0.8,1.2)) ;
#13413 = CARTESIAN_POINT('',(1.3,0.8,1.)) ;
#13414 = CARTESIAN_POINT('Origin',(2.,0.8,1.2)) ;
#13415 = CARTESIAN_POINT('Origin',(2.,0.8,1.2)) ;
#13416 = CARTESIAN_POINT('',(1.2,0.8,1.2)) ;
#13417 = CARTESIAN_POINT('Origin',(2.,0.8,1.2)) ;
#13418 = CARTESIAN_POINT('Origin',(2.,0.8,0.75)) ;
#13419 = CARTESIAN_POINT('',(1.2,0.8,0.7)) ;
#13420 = CARTESIAN_POINT('',(1.2,0.8,0.75)) ;
#13421 = CARTESIAN_POINT('Origin',(2.,0.8,0.7)) ;
#13422 = CARTESIAN_POINT('Origin',(2.,0.8,0.7)) ;
#13423 = CARTESIAN_POINT('Origin',(2.,0.8,0.8)) ;
#13424 = CARTESIAN_POINT('',(0.,0.,0.)) ;
#13425 = CARTESIAN_POINT('Origin',(2.,0.8,1.11)) ;
#13426 = CARTESIAN_POINT('',(1.8,0.8,1.13)) ;
#13427 = CARTESIAN_POINT('Origin',(2.,0.8,1.13)) ;
#13428 = CARTESIAN_POINT('',(1.8,0.8,1.09)) ;
#13429 = CARTESIAN_POINT('',(1.8,0.8,1.11)) ;
#13430 = CARTESIAN_POINT('Origin',(2.,0.8,1.09)) ;
#13431 = CARTESIAN_POINT('Origin',(2.,0.8,1.13)) ;
#13432 = CARTESIAN_POINT('Origin',(2.,0.8,1.07)) ;
#13433 = CARTESIAN_POINT('',(1.31,0.8,1.09)) ;
#13434 = CARTESIAN_POINT('Origin',(2.,0.8,1.09)) ;
#13435 = CARTESIAN_POINT('',(1.31,0.8,1.05)) ;
#13436 = CARTESIAN_POINT('',(1.31,0.8,1.07)) ;
#13437 = CARTESIAN_POINT('Origin',(2.,0.8,1.05)) ;
#13438 = CARTESIAN_POINT('Origin',(2.,0.8,1.05)) ;
#13439 = CARTESIAN_POINT('Origin',(2.,0.8,1.09)) ;
#13440 = CARTESIAN_POINT('',(0.,0.,0.)) ;
#13441 = CARTESIAN_POINT('Origin',(2.,0.8,1.64)) ;
#13442 = CARTESIAN_POINT('',(1.88,0.8,2.15)) ;
#13443 = CARTESIAN_POINT('Origin',(2.,0.8,2.15)) ;
#13444 = CARTESIAN_POINT('',(1.88,0.8,1.13)) ;
#13445 = CARTESIAN_POINT('',(1.88,0.8,1.64)) ;
#13446 = CARTESIAN_POINT('Origin',(2.,0.8,1.13)) ;
#13447 = CARTESIAN_POINT('Origin',(2.,0.8,1.13)) ;
#13448 = CARTESIAN_POINT('Origin',(2.,0.8,2.15)) ;
#13449 = CARTESIAN_POINT('',(0.,0.,0.)) ;
#13450 = CARTESIAN_POINT('Origin',(2.15,1.4,1.56)) ;
#13451 = CARTESIAN_POINT('',(2.15,1.5959899496853,1.52)) ;
#13452 = CARTESIAN_POINT('',(2.15,1.5959899496853,1.6)) ;
#13453 = CARTESIAN_POINT('',(2.15,1.5959899496853,1.5)) ;
#13454 = CARTESIAN_POINT('',(2.15,1.05,1.52)) ;
#13455 = CARTESIAN_POINT('',(2.15,1.4,1.52)) ;
#13456 = CARTESIAN_POINT('',(2.15,1.05,1.6)) ;
#13457 = CARTESIAN_POINT('',(2.15,1.05,1.56)) ;
#13458 = CARTESIAN_POINT('',(2.15,1.4,1.6)) ;
#13459 = CARTESIAN_POINT('Origin',(2.5,1.4,1.6)) ;
#13460 = CARTESIAN_POINT('',(2.85,1.64705371730487,1.6)) ;
#13461 = CARTESIAN_POINT('',(2.73314391493076,1.75,1.6)) ;
#13462 = CARTESIAN_POINT('Origin',(2.,0.8,1.6)) ;
#13463 = CARTESIAN_POINT('',(2.85,1.75,1.6)) ;
#13464 = CARTESIAN_POINT('',(2.85,1.4,1.6)) ;
#13465 = CARTESIAN_POINT('',(2.5,1.75,1.6)) ;
#13466 = CARTESIAN_POINT('Origin',(2.85,1.4,1.56)) ;
#13467 = CARTESIAN_POINT('',(2.85,1.64705371730487,1.52)) ;
#13468 = CARTESIAN_POINT('',(2.85,1.64705371730487,1.5)) ;
#13469 = CARTESIAN_POINT('',(2.85,1.75,1.52)) ;
#13470 = CARTESIAN_POINT('',(2.85,1.4,1.52)) ;
#13471 = CARTESIAN_POINT('',(2.85,1.75,1.56)) ;
#13472 = CARTESIAN_POINT('Origin',(2.5,1.4,1.52)) ;
#13473 = CARTESIAN_POINT('',(2.73314391493076,1.75,1.52)) ;
#13474 = CARTESIAN_POINT('Origin',(2.,0.8,1.52)) ;
#13475 = CARTESIAN_POINT('',(2.5,1.75,1.52)) ;
#13476 = CARTESIAN_POINT('Origin',(2.5,1.4,1.52)) ;
#13477 = CARTESIAN_POINT('',(2.77045441137033,1.05,1.52)) ;
#13478 = CARTESIAN_POINT('Origin',(2.,0.8,1.52)) ;
#13479 = CARTESIAN_POINT('',(2.5,1.05,1.52)) ;
#13480 = CARTESIAN_POINT('Origin',(2.5,1.4,1.6)) ;
#13481 = CARTESIAN_POINT('',(2.77045441137033,1.05,1.6)) ;
#13482 = CARTESIAN_POINT('Origin',(2.,0.8,1.6)) ;
#13483 = CARTESIAN_POINT('',(2.5,1.05,1.6)) ;
#13484 = CARTESIAN_POINT('Origin',(2.5,1.05,1.56)) ;
#13485 = CARTESIAN_POINT('',(2.77045441137033,1.05,1.5)) ;
#13486 = CARTESIAN_POINT('Origin',(2.5,1.75,1.56)) ;
#13487 = CARTESIAN_POINT('',(2.73314391493076,1.75,1.5)) ;
#13488 = CARTESIAN_POINT('Origin',(2.,0.8,1.9)) ;
#13489 = CARTESIAN_POINT('',(1.87,0.8,1.8)) ;
#13490 = CARTESIAN_POINT('Origin',(2.,0.8,1.8)) ;
#13491 = CARTESIAN_POINT('',(1.87,0.8,2.)) ;
#13492 = CARTESIAN_POINT('',(1.87,0.8,1.9)) ;
#13493 = CARTESIAN_POINT('Origin',(2.,0.8,2.)) ;
#13494 = CARTESIAN_POINT('Origin',(2.5,1.4,1.7)) ;
#13495 = CARTESIAN_POINT('',(2.75920310052949,1.08233074955876,1.7)) ;
#13496 = CARTESIAN_POINT('',(2.14079689947051,1.59766925044124,1.7)) ;
#13497 = CARTESIAN_POINT('Origin',(2.,0.8,1.7)) ;
#13498 = CARTESIAN_POINT('Origin',(2.5,1.4,1.7)) ;
#13499 = CARTESIAN_POINT('Origin',(2.5,1.4,1.9)) ;
#13500 = CARTESIAN_POINT('',(2.75920310052949,1.08233074955876,1.8)) ;
#13501 = CARTESIAN_POINT('',(2.75920310052949,1.08233074955876,1.9)) ;
#13502 = CARTESIAN_POINT('',(2.09,1.4,1.8)) ;
#13503 = CARTESIAN_POINT('Origin',(2.5,1.4,1.8)) ;
#13504 = CARTESIAN_POINT('',(2.09,1.4,2.)) ;
#13505 = CARTESIAN_POINT('',(2.09,1.4,1.9)) ;
#13506 = CARTESIAN_POINT('Origin',(2.5,1.4,2.)) ;
#13507 = CARTESIAN_POINT('',(2.14079689947051,1.59766925044124,1.8)) ;
#13508 = CARTESIAN_POINT('Origin',(2.5,1.4,1.8)) ;
#13509 = CARTESIAN_POINT('',(2.14079689947051,1.59766925044124,1.9)) ;
#13510 = CARTESIAN_POINT('Origin',(2.,0.8,1.5)) ;
#13511 = CARTESIAN_POINT('',(1.19,0.8,1.2)) ;
#13512 = CARTESIAN_POINT('Origin',(2.,0.8,1.2)) ;
#13513 = CARTESIAN_POINT('',(1.19,0.8,1.8)) ;
#13514 = CARTESIAN_POINT('',(1.19,0.8,1.5)) ;
#13515 = CARTESIAN_POINT('Origin',(2.,0.8,1.8)) ;
#13516 = CARTESIAN_POINT('Origin',(2.,0.8,1.8)) ;
#13517 = CARTESIAN_POINT('Origin',(2.,0.8,1.8)) ;
#13518 = CARTESIAN_POINT('Origin',(2.,0.8,2.)) ;
#13519 = CARTESIAN_POINT('',(0.8,0.8,2.)) ;
#13520 = CARTESIAN_POINT('Origin',(2.,0.8,2.)) ;
#13521 = CARTESIAN_POINT('Origin',(2.,0.8,1.5)) ;
#13522 = CARTESIAN_POINT('',(0.8,0.8,1.2)) ;
#13523 = CARTESIAN_POINT('',(0.8,0.8,1.5)) ;
#13524 = CARTESIAN_POINT('Origin',(2.,0.8,1.2)) ;
#13525 = CARTESIAN_POINT('Origin',(2.,0.8,1.2)) ;
#13526 = CARTESIAN_POINT('',(0.,0.,0.)) ;
#13527 = CARTESIAN_POINT('Origin',(2.5,1.4,3.4)) ;
#13528 = CARTESIAN_POINT('',(2.5,1.4,3.1)) ;
#13529 = CARTESIAN_POINT('',(2.5,1.4,3.7)) ;
#13530 = CARTESIAN_POINT('Origin',(2.5,1.4,3.4)) ;
#13531 = CARTESIAN_POINT('Origin',(2.5,1.4,3.4)) ;
#13532 = CARTESIAN_POINT('',(2.76457513110646,1.54142135623731,3.13542486889354)) ;
#13533 = CARTESIAN_POINT('',(2.76457513110646,1.25857864376269,3.13542486889354)) ;
#13534 = CARTESIAN_POINT('Origin',(2.76457513110646,1.4,3.4)) ;
#13535 = CARTESIAN_POINT('Origin',(2.5,1.4,3.13542486889354)) ;
#13536 = CARTESIAN_POINT('Origin',(2.5,1.4,2.55)) ;
#13537 = CARTESIAN_POINT('Origin',(2.5,1.4,3.4)) ;
#13538 = CARTESIAN_POINT('Origin',(3.15,1.4,3.4)) ;
#13539 = CARTESIAN_POINT('Origin',(2.5,1.4,1.7)) ;
#13540 = CARTESIAN_POINT('',(2.1,1.4,1.7)) ;
#13541 = CARTESIAN_POINT('Origin',(2.5,1.4,1.7)) ;
#13542 = CARTESIAN_POINT('',(2.2,1.4,1.7)) ;
#13543 = CARTESIAN_POINT('Origin',(2.5,1.4,1.7)) ;
#13544 = CARTESIAN_POINT('Origin',(2.5,1.4,2.55)) ;
#13545 = CARTESIAN_POINT('',(2.76457513110646,1.1,3.4)) ;
#13546 = CARTESIAN_POINT('',(2.76457513110646,1.7,3.4)) ;
#13547 = CARTESIAN_POINT('Ctrl Pts',(2.76457513110646,1.1,3.4)) ;
#13548 = CARTESIAN_POINT('Ctrl Pts',(2.76457513110646,1.1,3.37985532278493)) ;
#13549 = CARTESIAN_POINT('Ctrl Pts',(2.76694665658319,1.1020492278835,3.3596364158444)) ;
#13550 = CARTESIAN_POINT('Ctrl Pts',(2.7756634705603,1.11009513514317,3.32025634008317)) ;
#13551 = CARTESIAN_POINT('Ctrl Pts',(2.78197027038471,1.11608711674642,3.30108570205275)) ;
#13552 = CARTESIAN_POINT('Ctrl Pts',(2.80406356980255,1.1392312552828,3.24650091982942)) ;
#13553 = CARTESIAN_POINT('Ctrl Pts',(2.82281865282694,1.16181405724795,3.21392187404012)) ;
#13554 = CARTESIAN_POINT('Ctrl Pts',(2.85507155223138,1.21337388114196,3.16236205014611)) ;
#13555 = CARTESIAN_POINT('Ctrl Pts',(2.87117243484146,1.24601764444721,3.13945139911714)) ;
#13556 = CARTESIAN_POINT('Ctrl Pts',(2.89371396047987,1.31957074694018,3.10823419970573)) ;
#13557 = CARTESIAN_POINT('Ctrl Pts',(2.9,1.36055805317426,3.1)) ;
#13558 = CARTESIAN_POINT('Ctrl Pts',(2.9,1.43944194682574,3.1)) ;
#13559 = CARTESIAN_POINT('Ctrl Pts',(2.89371396047987,1.48042925305982,3.10823419970573)) ;
#13560 = CARTESIAN_POINT('Ctrl Pts',(2.87117243484146,1.55398235555279,3.13945139911714)) ;
#13561 = CARTESIAN_POINT('Ctrl Pts',(2.85507155223138,1.58662611885804,3.16236205014611)) ;
#13562 = CARTESIAN_POINT('Ctrl Pts',(2.82281865282694,1.63818594275205,3.21392187404012)) ;
#13563 = CARTESIAN_POINT('Ctrl Pts',(2.80406356980255,1.6607687447172,3.24650091982942)) ;
#13564 = CARTESIAN_POINT('Ctrl Pts',(2.78197027038471,1.68391288325358,3.30108570205275)) ;
#13565 = CARTESIAN_POINT('Ctrl Pts',(2.7756634705603,1.68990486485683,3.32025634008317)) ;
#13566 = CARTESIAN_POINT('Ctrl Pts',(2.76694665658319,1.6979507721165,3.3596364158444)) ;
#13567 = CARTESIAN_POINT('Ctrl Pts',(2.76457513110646,1.7,3.37985532278493)) ;
#13568 = CARTESIAN_POINT('Ctrl Pts',(2.76457513110646,1.7,3.4)) ;
#13569 = CARTESIAN_POINT('Origin',(2.5,1.4,3.4)) ;
#13570 = CARTESIAN_POINT('Origin',(2.5,1.4,2.55)) ;
#13571 = CARTESIAN_POINT('',(2.5,1.8,3.4)) ;
#13572 = CARTESIAN_POINT('',(2.5,1.,3.4)) ;
#13573 = CARTESIAN_POINT('Origin',(2.5,1.4,3.4)) ;
#13574 = CARTESIAN_POINT('',(2.1,1.4,3.4)) ;
#13575 = CARTESIAN_POINT('Origin',(2.5,1.4,3.4)) ;
#13576 = CARTESIAN_POINT('',(2.1,1.4,2.55)) ;
#13577 = CARTESIAN_POINT('Origin',(2.5,1.4,3.4)) ;
#13578 = CARTESIAN_POINT('Origin',(3.8,1.4,3.4)) ;
#13579 = CARTESIAN_POINT('',(3.8,1.4,3.8)) ;
#13580 = CARTESIAN_POINT('Origin',(3.8,1.4,3.4)) ;
#13581 = CARTESIAN_POINT('',(3.8,1.4,3.7)) ;
#13582 = CARTESIAN_POINT('Origin',(3.8,1.4,3.4)) ;
#13583 = CARTESIAN_POINT('Origin',(3.15,1.4,3.4)) ;
#13584 = CARTESIAN_POINT('',(2.5,1.1,3.13542486889354)) ;
#13585 = CARTESIAN_POINT('',(2.5,1.7,3.13542486889354)) ;
#13586 = CARTESIAN_POINT('Ctrl Pts',(2.5,1.1,3.13542486889354)) ;
#13587 = CARTESIAN_POINT('Ctrl Pts',(2.52014467721507,1.1,3.13542486889354)) ;
#13588 = CARTESIAN_POINT('Ctrl Pts',(2.5403635841556,1.1020492278835,3.13305334341681)) ;
#13589 = CARTESIAN_POINT('Ctrl Pts',(2.57974365991683,1.11009513514317,3.1243365294397)) ;
#13590 = CARTESIAN_POINT('Ctrl Pts',(2.59891429794725,1.11608711674642,3.11802972961529)) ;
#13591 = CARTESIAN_POINT('Ctrl Pts',(2.65349908017058,1.1392312552828,3.09593643019745)) ;
#13592 = CARTESIAN_POINT('Ctrl Pts',(2.68607812595988,1.16181405724795,3.07718134717306)) ;
#13593 = CARTESIAN_POINT('Ctrl Pts',(2.73763794985389,1.21337388114196,3.04492844776862)) ;
#13594 = CARTESIAN_POINT('Ctrl Pts',(2.76054860088286,1.24601764444721,3.02882756515854)) ;
#13595 = CARTESIAN_POINT('Ctrl Pts',(2.79176580029427,1.31957074694018,3.00628603952013)) ;
#13596 = CARTESIAN_POINT('Ctrl Pts',(2.8,1.36055805317426,3.)) ;
#13597 = CARTESIAN_POINT('Ctrl Pts',(2.8,1.43944194682574,3.)) ;
#13598 = CARTESIAN_POINT('Ctrl Pts',(2.79176580029427,1.48042925305982,3.00628603952013)) ;
#13599 = CARTESIAN_POINT('Ctrl Pts',(2.76054860088286,1.55398235555279,3.02882756515854)) ;
#13600 = CARTESIAN_POINT('Ctrl Pts',(2.73763794985389,1.58662611885804,3.04492844776862)) ;
#13601 = CARTESIAN_POINT('Ctrl Pts',(2.68607812595988,1.63818594275205,3.07718134717306)) ;
#13602 = CARTESIAN_POINT('Ctrl Pts',(2.65349908017058,1.6607687447172,3.09593643019745)) ;
#13603 = CARTESIAN_POINT('Ctrl Pts',(2.59891429794725,1.68391288325358,3.11802972961529)) ;
#13604 = CARTESIAN_POINT('Ctrl Pts',(2.57974365991683,1.68990486485683,3.1243365294397)) ;
#13605 = CARTESIAN_POINT('Ctrl Pts',(2.5403635841556,1.6979507721165,3.13305334341681)) ;
#13606 = CARTESIAN_POINT('Ctrl Pts',(2.52014467721507,1.7,3.13542486889354)) ;
#13607 = CARTESIAN_POINT('Ctrl Pts',(2.5,1.7,3.13542486889354)) ;
#13608 = CARTESIAN_POINT('Origin',(2.5,1.4,3.4)) ;
#13609 = CARTESIAN_POINT('Origin',(3.15,1.4,3.4)) ;
#13610 = CARTESIAN_POINT('',(2.5,1.4,3.8)) ;
#13611 = CARTESIAN_POINT('',(3.15,1.4,3.8)) ;
#13612 = CARTESIAN_POINT('Origin',(2.5,1.4,3.4)) ;
#13613 = CARTESIAN_POINT('Origin',(2.5,1.4,3.4)) ;
#13614 = CARTESIAN_POINT('Origin',(3.15,1.4,3.4)) ;
#13615 = CARTESIAN_POINT('',(2.76457513110646,1.4,3.7)) ;
#13616 = CARTESIAN_POINT('Origin',(2.76457513110646,1.4,3.4)) ;
#13617 = CARTESIAN_POINT('',(3.15,1.4,3.7)) ;
#13618 = CARTESIAN_POINT('Origin',(2.76457513110646,1.4,3.4)) ;
#13619 = CARTESIAN_POINT('Origin',(2.5,1.4,2.55)) ;
#13620 = CARTESIAN_POINT('',(2.2,1.4,3.13542486889354)) ;
#13621 = CARTESIAN_POINT('',(2.2,1.4,2.55)) ;
#13622 = CARTESIAN_POINT('Origin',(2.5,1.4,3.13542486889354)) ;
#13623 = CARTESIAN_POINT('Origin',(2.5,1.4,3.13542486889354)) ;
#13624 = CARTESIAN_POINT('Origin',(2.5,1.4,3.4)) ;
#13625 = CARTESIAN_POINT('Origin',(2.5,1.4,3.4)) ;
#13626 = CARTESIAN_POINT('Origin',(2.5,1.4,3.4)) ;
#13627 = CARTESIAN_POINT('',(0.,0.,0.)) ;
#13628 = CARTESIAN_POINT('Origin',(2.5,1.4,2.15)) ;
#13629 = CARTESIAN_POINT('',(2.1,1.4,2.)) ;
#13630 = CARTESIAN_POINT('Origin',(2.5,1.4,2.)) ;
#13631 = CARTESIAN_POINT('',(2.1,1.4,2.3)) ;
#13632 = CARTESIAN_POINT('',(2.1,1.4,2.15)) ;
#13633 = CARTESIAN_POINT('Origin',(2.5,1.4,2.3)) ;
#13634 = CARTESIAN_POINT('Origin',(2.5,1.4,2.15)) ;
#13635 = CARTESIAN_POINT('',(2.05,1.4,2.3)) ;
#13636 = CARTESIAN_POINT('Origin',(2.5,1.4,2.3)) ;
#13637 = CARTESIAN_POINT('',(2.05,1.4,2.)) ;
#13638 = CARTESIAN_POINT('',(2.05,1.4,2.15)) ;
#13639 = CARTESIAN_POINT('Origin',(2.5,1.4,2.)) ;
#13640 = CARTESIAN_POINT('Origin',(2.5,1.4,2.)) ;
#13641 = CARTESIAN_POINT('Origin',(2.5,1.4,2.3)) ;
#13642 = CARTESIAN_POINT('',(0.,0.,0.)) ;
#13643 = CARTESIAN_POINT('Origin',(0.,-1.4,1.15)) ;
#13644 = CARTESIAN_POINT('',(-0.13,-1.4,1.1)) ;
#13645 = CARTESIAN_POINT('Origin',(0.,-1.4,1.1)) ;
#13646 = CARTESIAN_POINT('',(-0.13,-1.4,1.2)) ;
#13647 = CARTESIAN_POINT('',(-0.13,-1.4,1.15)) ;
#13648 = CARTESIAN_POINT('Origin',(0.,-1.4,1.2)) ;
#13649 = CARTESIAN_POINT('Origin',(0.,-1.4,1.35)) ;
#13650 = CARTESIAN_POINT('',(-0.71,-1.4,1.2)) ;
#13651 = CARTESIAN_POINT('Origin',(0.,-1.4,1.2)) ;
#13652 = CARTESIAN_POINT('',(-0.71,-1.4,1.5)) ;
#13653 = CARTESIAN_POINT('',(-0.71,-1.4,1.35)) ;
#13654 = CARTESIAN_POINT('Origin',(0.,-1.4,1.5)) ;
#13655 = CARTESIAN_POINT('Origin',(0.,-1.4,1.5)) ;
#13656 = CARTESIAN_POINT('',(-0.85,-1.4,1.5)) ;
#13657 = CARTESIAN_POINT('Origin',(0.,-1.4,1.5)) ;
#13658 = CARTESIAN_POINT('Origin',(0.,-1.4,1.15)) ;
#13659 = CARTESIAN_POINT('',(-0.85,-1.4,1.1)) ;
#13660 = CARTESIAN_POINT('',(-0.85,-1.4,1.15)) ;
#13661 = CARTESIAN_POINT('Origin',(0.,-1.4,1.1)) ;
#13662 = CARTESIAN_POINT('Origin',(0.,-1.4,1.1)) ;
#13663 = CARTESIAN_POINT('Origin',(0.,-1.4,1.2)) ;
#13664 = CARTESIAN_POINT('',(0.,0.,0.)) ;
#13665 = CARTESIAN_POINT('Origin',(0.,-1.4,1.27)) ;
#13666 = CARTESIAN_POINT('',(-0.7,-1.4,1.29)) ;
#13667 = CARTESIAN_POINT('Origin',(0.,-1.4,1.29)) ;
#13668 = CARTESIAN_POINT('',(-0.7,-1.4,1.25)) ;
#13669 = CARTESIAN_POINT('',(-0.7,-1.4,1.27)) ;
#13670 = CARTESIAN_POINT('Origin',(0.,-1.4,1.25)) ;
#13671 = CARTESIAN_POINT('Origin',(0.,-1.4,1.25)) ;
#13672 = CARTESIAN_POINT('Origin',(0.,-1.4,1.29)) ;
#13673 = CARTESIAN_POINT('',(0.,0.,0.)) ;
#13674 = CARTESIAN_POINT('Origin',(0.,-1.4,0.825)) ;
#13675 = CARTESIAN_POINT('',(-0.12,-1.4,1.25)) ;
#13676 = CARTESIAN_POINT('Origin',(0.,-1.4,1.25)) ;
#13677 = CARTESIAN_POINT('',(-0.12,-1.4,0.4)) ;
#13678 = CARTESIAN_POINT('',(-0.12,-1.4,0.825)) ;
#13679 = CARTESIAN_POINT('Origin',(0.,-1.4,0.4)) ;
#13680 = CARTESIAN_POINT('Origin',(0.,-1.4,0.4)) ;
#13681 = CARTESIAN_POINT('Origin',(0.,-1.4,1.25)) ;
#13682 = CARTESIAN_POINT('',(0.,0.,0.)) ;
#13683 = CARTESIAN_POINT('',(0.,0.,0.)) ;
#13684 = CARTESIAN_POINT('',(0.,0.,0.)) ;
#13685 = CARTESIAN_POINT('',(0.,0.,0.)) ;
#13686 = CARTESIAN_POINT('',(0.,0.,0.)) ;
#13687 = CARTESIAN_POINT('',(0.,0.,0.)) ;
#13688 = CARTESIAN_POINT('',(0.,0.,0.)) ;
#13689 = CARTESIAN_POINT('',(0.,0.,0.)) ;
#13690 = CARTESIAN_POINT('',(0.,0.,0.)) ;
#13691 = CARTESIAN_POINT('',(0.,0.,0.)) ;
#13692 = CARTESIAN_POINT('',(0.,0.,0.)) ;
#13693 = CARTESIAN_POINT('Origin',(2.,0.7,2.3)) ;
#13694 = CARTESIAN_POINT('',(1.87,0.7,2.15)) ;
#13695 = CARTESIAN_POINT('Origin',(2.,0.7,2.15)) ;
#13696 = CARTESIAN_POINT('',(1.87,0.7,2.45)) ;
#13697 = CARTESIAN_POINT('',(1.87,0.7,2.3)) ;
#13698 = CARTESIAN_POINT('Origin',(2.,0.7,2.45)) ;
#13699 = CARTESIAN_POINT('Origin',(-2.45,0.7,1.7)) ;
#13700 = CARTESIAN_POINT('',(-2.3,0.9,1.7)) ;
#13701 = CARTESIAN_POINT('',(-2.3,0.5,1.7)) ;
#13702 = CARTESIAN_POINT('',(-2.3,0.7,1.7)) ;
#13703 = CARTESIAN_POINT('',(-2.6,0.5,1.7)) ;
#13704 = CARTESIAN_POINT('',(-2.45,0.5,1.7)) ;
#13705 = CARTESIAN_POINT('',(-2.6,0.9,1.7)) ;
#13706 = CARTESIAN_POINT('',(-2.6,0.7,1.7)) ;
#13707 = CARTESIAN_POINT('',(-2.45,0.9,1.7)) ;
#13708 = CARTESIAN_POINT('Origin',(-2.6,0.7,2.075)) ;
#13709 = CARTESIAN_POINT('',(-2.6,0.9,2.45)) ;
#13710 = CARTESIAN_POINT('',(-2.6,0.9,2.075)) ;
#13711 = CARTESIAN_POINT('',(-2.6,0.5,2.45)) ;
#13712 = CARTESIAN_POINT('',(-2.6,0.5,2.075)) ;
#13713 = CARTESIAN_POINT('',(-2.6,0.7,2.45)) ;
#13714 = CARTESIAN_POINT('Origin',(-2.3,0.7,2.075)) ;
#13715 = CARTESIAN_POINT('',(-2.3,0.5,2.15)) ;
#13716 = CARTESIAN_POINT('',(-2.3,0.9,2.15)) ;
#13717 = CARTESIAN_POINT('',(-2.3,0.7,2.15)) ;
#13718 = CARTESIAN_POINT('',(-2.3,0.5,2.075)) ;
#13719 = CARTESIAN_POINT('',(-2.3,0.9,2.075)) ;
#13720 = CARTESIAN_POINT('Origin',(-0.1,0.5,2.3)) ;
#13721 = CARTESIAN_POINT('',(0.340192378864668,0.5,2.15)) ;
#13722 = CARTESIAN_POINT('',(-0.1,0.5,2.15)) ;
#13723 = CARTESIAN_POINT('',(0.859807621135332,0.5,2.15)) ;
#13724 = CARTESIAN_POINT('Origin',(0.6,0.5,2.3)) ;
#13725 = CARTESIAN_POINT('',(2.2,0.5,2.15)) ;
#13726 = CARTESIAN_POINT('',(-0.1,0.5,2.15)) ;
#13727 = CARTESIAN_POINT('',(2.2,0.5,2.45)) ;
#13728 = CARTESIAN_POINT('',(2.2,0.5,2.3)) ;
#13729 = CARTESIAN_POINT('',(0.859807621135332,0.5,2.45)) ;
#13730 = CARTESIAN_POINT('',(-0.1,0.5,2.45)) ;
#13731 = CARTESIAN_POINT('',(0.340192378864668,0.5,2.45)) ;
#13732 = CARTESIAN_POINT('Origin',(0.6,0.5,2.3)) ;
#13733 = CARTESIAN_POINT('',(-0.1,0.5,2.45)) ;
#13734 = CARTESIAN_POINT('',(0.47,0.5,2.3)) ;
#13735 = CARTESIAN_POINT('Origin',(0.6,0.5,2.3)) ;
#13736 = CARTESIAN_POINT('Origin',(-0.1,0.7,2.15)) ;
#13737 = CARTESIAN_POINT('',(0.340192378864668,0.9,2.15)) ;
#13738 = CARTESIAN_POINT('',(-0.1,0.9,2.15)) ;
#13739 = CARTESIAN_POINT('',(0.340192378864668,0.7,2.15)) ;
#13740 = CARTESIAN_POINT('Origin',(0.6,0.7,2.3)) ;
#13741 = CARTESIAN_POINT('',(0.47,0.9,2.3)) ;
#13742 = CARTESIAN_POINT('',(0.47,0.7,2.3)) ;
#13743 = CARTESIAN_POINT('Origin',(0.6,0.9,2.3)) ;
#13744 = CARTESIAN_POINT('Origin',(0.6,0.7,2.3)) ;
#13745 = CARTESIAN_POINT('',(0.859807621135332,0.9,2.15)) ;
#13746 = CARTESIAN_POINT('Origin',(0.6,0.9,2.3)) ;
#13747 = CARTESIAN_POINT('',(0.859807621135332,0.7,2.15)) ;
#13748 = CARTESIAN_POINT('Origin',(0.6,0.7,2.3)) ;
#13749 = CARTESIAN_POINT('',(0.340192378864668,0.9,2.45)) ;
#13750 = CARTESIAN_POINT('',(0.340192378864668,0.7,2.45)) ;
#13751 = CARTESIAN_POINT('',(0.859807621135332,0.9,2.45)) ;
#13752 = CARTESIAN_POINT('',(0.859807621135332,0.7,2.45)) ;
#13753 = CARTESIAN_POINT('Origin',(0.6,0.9,2.3)) ;
#13754 = CARTESIAN_POINT('Origin',(-0.1,0.7,2.45)) ;
#13755 = CARTESIAN_POINT('',(2.2,0.9,2.45)) ;
#13756 = CARTESIAN_POINT('',(2.2,0.7,2.45)) ;
#13757 = CARTESIAN_POINT('',(-0.1,0.9,2.45)) ;
#13758 = CARTESIAN_POINT('Origin',(-0.1,0.7,2.45)) ;
#13759 = CARTESIAN_POINT('',(-0.1,0.9,2.45)) ;
#13760 = CARTESIAN_POINT('Origin',(-0.1,0.9,2.3)) ;
#13761 = CARTESIAN_POINT('',(2.2,0.9,2.15)) ;
#13762 = CARTESIAN_POINT('',(2.2,0.9,2.3)) ;
#13763 = CARTESIAN_POINT('',(-0.1,0.9,2.15)) ;
#13764 = CARTESIAN_POINT('Origin',(-0.1,0.7,2.15)) ;
#13765 = CARTESIAN_POINT('',(2.2,0.7,2.15)) ;
#13766 = CARTESIAN_POINT('Origin',(2.2,0.7,2.3)) ;
#13767 = CARTESIAN_POINT('',(0.,0.,0.)) ;
#13768 = CARTESIAN_POINT('Origin',(0.6,0.,2.3)) ;
#13769 = CARTESIAN_POINT('',(0.4,0.,2.3)) ;
#13770 = CARTESIAN_POINT('Origin',(0.6,0.,2.3)) ;
#13771 = CARTESIAN_POINT('',(0.475,0.,2.3)) ;
#13772 = CARTESIAN_POINT('Origin',(0.6,0.,2.3)) ;
#13773 = CARTESIAN_POINT('Origin',(0.6,-0.05,2.3)) ;
#13774 = CARTESIAN_POINT('',(0.4,-0.1,2.3)) ;
#13775 = CARTESIAN_POINT('',(0.4,-0.05,2.3)) ;
#13776 = CARTESIAN_POINT('Origin',(0.6,-0.1,2.3)) ;
#13777 = CARTESIAN_POINT('Origin',(0.6,-0.1,2.3)) ;
#13778 = CARTESIAN_POINT('Origin',(0.6,0.7,2.3)) ;
#13779 = CARTESIAN_POINT('',(0.475,1.4,2.3)) ;
#13780 = CARTESIAN_POINT('Origin',(0.6,1.4,2.3)) ;
#13781 = CARTESIAN_POINT('',(0.475,0.7,2.3)) ;
#13782 = CARTESIAN_POINT('Origin',(0.6,1.4,2.3)) ;
#13783 = CARTESIAN_POINT('',(0.,0.,0.)) ;
#13784 = CARTESIAN_POINT('Origin',(-1.32322330470336,0.523223304703363,1.87625)) ;
#13785 = CARTESIAN_POINT('',(-1.31990818206448,0.52653842734225,1.85169353600825)) ;
#13786 = CARTESIAN_POINT('',(-1.32653842734225,0.519908182064476,1.90080646399175)) ;
#13787 = CARTESIAN_POINT('Origin',(-1.32322330470336,0.523223304703363,1.87625)) ;
#13788 = CARTESIAN_POINT('Origin',(-1.32322330470336,0.523223304703363,1.87625)) ;
#13789 = CARTESIAN_POINT('Origin',(-1.5,0.45,1.8425)) ;
#13790 = CARTESIAN_POINT('',(-1.49531170860316,0.45,1.81794353600825)) ;
#13791 = CARTESIAN_POINT('',(-1.50468829139684,0.45,1.86705646399175)) ;
#13792 = CARTESIAN_POINT('Origin',(-1.5,0.45,1.8425)) ;
#13793 = CARTESIAN_POINT('',(-1.51037428027778,0.429342812247576,1.85202128682895)) ;
#13794 = CARTESIAN_POINT('Origin',(-1.5,0.45,1.8425)) ;
#13795 = CARTESIAN_POINT('Origin',(-1.5,0.45,1.8425)) ;
#13796 = CARTESIAN_POINT('Origin',(-1.67677669529664,0.523223304703363,1.80875)) ;
#13797 = CARTESIAN_POINT('',(-1.67346157265775,0.519908182064476,1.78419353600825)) ;
#13798 = CARTESIAN_POINT('',(-1.68715097557442,0.502566116950939,1.81827128682895)) ;
#13799 = CARTESIAN_POINT('Origin',(-1.67677669529664,0.523223304703363,1.80875)) ;
#13800 = CARTESIAN_POINT('',(-1.68009181793552,0.52653842734225,1.83330646399175)) ;
#13801 = CARTESIAN_POINT('Origin',(-1.67677669529664,0.523223304703363,1.80875)) ;
#13802 = CARTESIAN_POINT('',(-1.69993339200128,0.513968813087923,1.81051685671998)) ;
#13803 = CARTESIAN_POINT('Origin',(-1.67677669529664,0.523223304703363,1.80875)) ;
#13804 = CARTESIAN_POINT('Origin',(-1.67677669529664,0.523223304703363,1.80875)) ;
#13805 = CARTESIAN_POINT('Origin',(-1.75,0.7,1.775)) ;
#13806 = CARTESIAN_POINT('',(-1.75,0.695311708603157,1.75044353600825)) ;
#13807 = CARTESIAN_POINT('',(-1.77315669670464,0.69074550838456,1.77676685671998)) ;
#13808 = CARTESIAN_POINT('Origin',(-1.75,0.7,1.775)) ;
#13809 = CARTESIAN_POINT('',(-1.75,0.704688291396844,1.79955646399175)) ;
#13810 = CARTESIAN_POINT('Origin',(-1.75,0.7,1.775)) ;
#13811 = CARTESIAN_POINT('',(-1.77315669670464,0.709254491615441,1.77323314328002)) ;
#13812 = CARTESIAN_POINT('Origin',(-1.75,0.7,1.775)) ;
#13813 = CARTESIAN_POINT('Origin',(-1.75,0.7,1.775)) ;
#13814 = CARTESIAN_POINT('Origin',(-1.67677669529664,0.876776695296637,1.74125)) ;
#13815 = CARTESIAN_POINT('',(-1.68009181793552,0.873461572657751,1.71669353600825)) ;
#13816 = CARTESIAN_POINT('',(-1.69993339200128,0.886031186912078,1.73948314328002)) ;
#13817 = CARTESIAN_POINT('Origin',(-1.67677669529664,0.876776695296637,1.74125)) ;
#13818 = CARTESIAN_POINT('',(-1.67346157265775,0.880091817935524,1.76580646399175)) ;
#13819 = CARTESIAN_POINT('Origin',(-1.67677669529664,0.876776695296637,1.74125)) ;
#13820 = CARTESIAN_POINT('',(-1.68715097557442,0.897433883049061,1.73172871317105)) ;
#13821 = CARTESIAN_POINT('Origin',(-1.67677669529664,0.876776695296637,1.74125)) ;
#13822 = CARTESIAN_POINT('Origin',(-1.67677669529664,0.876776695296637,1.74125)) ;
#13823 = CARTESIAN_POINT('Origin',(-1.5,0.95,1.7075)) ;
#13824 = CARTESIAN_POINT('',(-1.50468829139684,0.95,1.68294353600825)) ;
#13825 = CARTESIAN_POINT('',(-1.51037428027778,0.970657187752424,1.69797871317105)) ;
#13826 = CARTESIAN_POINT('Origin',(-1.5,0.95,1.7075)) ;
#13827 = CARTESIAN_POINT('',(-1.49531170860316,0.95,1.73205646399175)) ;
#13828 = CARTESIAN_POINT('Origin',(-1.5,0.95,1.7075)) ;
#13829 = CARTESIAN_POINT('Origin',(-1.5,0.95,1.7075)) ;
#13830 = CARTESIAN_POINT('Origin',(-1.32322330470336,0.876776695296637,1.67375)) ;
#13831 = CARTESIAN_POINT('',(-1.32653842734225,0.880091817935524,1.64919353600825)) ;
#13832 = CARTESIAN_POINT('',(-1.31990818206448,0.87346157265775,1.69830646399175)) ;
#13833 = CARTESIAN_POINT('Origin',(-1.32322330470336,0.876776695296637,1.67375)) ;
#13834 = CARTESIAN_POINT('Origin',(-1.32322330470336,0.876776695296637,1.67375)) ;
#13835 = CARTESIAN_POINT('Origin',(-1.25,0.7,1.64)) ;
#13836 = CARTESIAN_POINT('',(-1.25,0.704688291396843,1.61544353600825)) ;
#13837 = CARTESIAN_POINT('',(-1.25,0.695311708603156,1.66455646399175)) ;
#13838 = CARTESIAN_POINT('Origin',(-1.25,0.7,1.64)) ;
#13839 = CARTESIAN_POINT('Origin',(-1.25,0.7,1.64)) ;
#13840 = CARTESIAN_POINT('Origin',(-1.32322330470336,0.523223304703363,1.60625)) ;
#13841 = CARTESIAN_POINT('',(-1.31990818206448,0.52653842734225,1.58169353600825)) ;
#13842 = CARTESIAN_POINT('',(-1.32653842734225,0.519908182064476,1.63080646399175)) ;
#13843 = CARTESIAN_POINT('Origin',(-1.32322330470336,0.523223304703363,1.60625)) ;
#13844 = CARTESIAN_POINT('Origin',(-1.32322330470336,0.523223304703363,1.60625)) ;
#13845 = CARTESIAN_POINT('Origin',(-1.5,0.45,1.5725)) ;
#13846 = CARTESIAN_POINT('',(-1.49531170860316,0.45,1.54794353600825)) ;
#13847 = CARTESIAN_POINT('',(-1.50468829139684,0.45,1.59705646399175)) ;
#13848 = CARTESIAN_POINT('Origin',(-1.5,0.45,1.5725)) ;
#13849 = CARTESIAN_POINT('',(-1.51037428027778,0.429342812247576,1.58202128682895)) ;
#13850 = CARTESIAN_POINT('Origin',(-1.5,0.45,1.5725)) ;
#13851 = CARTESIAN_POINT('Origin',(-1.5,0.45,1.5725)) ;
#13852 = CARTESIAN_POINT('Origin',(-1.67677669529664,0.523223304703363,1.53875)) ;
#13853 = CARTESIAN_POINT('',(-1.67346157265775,0.519908182064476,1.51419353600825)) ;
#13854 = CARTESIAN_POINT('',(-1.68715097557442,0.502566116950939,1.54827128682895)) ;
#13855 = CARTESIAN_POINT('Origin',(-1.67677669529664,0.523223304703363,1.53875)) ;
#13856 = CARTESIAN_POINT('',(-1.68009181793552,0.52653842734225,1.56330646399175)) ;
#13857 = CARTESIAN_POINT('Origin',(-1.67677669529664,0.523223304703363,1.53875)) ;
#13858 = CARTESIAN_POINT('',(-1.69993339200128,0.513968813087923,1.54051685671998)) ;
#13859 = CARTESIAN_POINT('Origin',(-1.67677669529664,0.523223304703363,1.53875)) ;
#13860 = CARTESIAN_POINT('Origin',(-1.67677669529664,0.523223304703363,1.53875)) ;
#13861 = CARTESIAN_POINT('Origin',(-1.75,0.7,1.505)) ;
#13862 = CARTESIAN_POINT('',(-1.75,0.695311708603156,1.48044353600825)) ;
#13863 = CARTESIAN_POINT('',(-1.77315669670464,0.69074550838456,1.50676685671998)) ;
#13864 = CARTESIAN_POINT('Origin',(-1.75,0.7,1.505)) ;
#13865 = CARTESIAN_POINT('',(-1.75,0.704688291396844,1.52955646399175)) ;
#13866 = CARTESIAN_POINT('Origin',(-1.75,0.7,1.505)) ;
#13867 = CARTESIAN_POINT('',(-1.77315669670464,0.709254491615441,1.50323314328002)) ;
#13868 = CARTESIAN_POINT('Origin',(-1.75,0.7,1.505)) ;
#13869 = CARTESIAN_POINT('Origin',(-1.75,0.7,1.505)) ;
#13870 = CARTESIAN_POINT('Origin',(-1.67677669529664,0.876776695296637,1.47125)) ;
#13871 = CARTESIAN_POINT('',(-1.68009181793552,0.87346157265775,1.44669353600825)) ;
#13872 = CARTESIAN_POINT('',(-1.69993339200128,0.886031186912078,1.46948314328002)) ;
#13873 = CARTESIAN_POINT('Origin',(-1.67677669529664,0.876776695296637,1.47125)) ;
#13874 = CARTESIAN_POINT('',(-1.67346157265775,0.880091817935524,1.49580646399175)) ;
#13875 = CARTESIAN_POINT('Origin',(-1.67677669529664,0.876776695296637,1.47125)) ;
#13876 = CARTESIAN_POINT('',(-1.68715097557442,0.897433883049061,1.46172871317105)) ;
#13877 = CARTESIAN_POINT('Origin',(-1.67677669529664,0.876776695296637,1.47125)) ;
#13878 = CARTESIAN_POINT('Origin',(-1.67677669529664,0.876776695296637,1.47125)) ;
#13879 = CARTESIAN_POINT('Origin',(-1.5,0.95,1.4375)) ;
#13880 = CARTESIAN_POINT('',(-1.50468829139684,0.95,1.41294353600825)) ;
#13881 = CARTESIAN_POINT('',(-1.51037428027778,0.970657187752424,1.42797871317105)) ;
#13882 = CARTESIAN_POINT('Origin',(-1.5,0.95,1.4375)) ;
#13883 = CARTESIAN_POINT('',(-1.49531170860316,0.95,1.46205646399175)) ;
#13884 = CARTESIAN_POINT('Origin',(-1.5,0.95,1.4375)) ;
#13885 = CARTESIAN_POINT('Origin',(-1.5,0.95,1.4375)) ;
#13886 = CARTESIAN_POINT('Origin',(-1.32322330470336,0.876776695296637,1.40375)) ;
#13887 = CARTESIAN_POINT('',(-1.32653842734225,0.880091817935524,1.37919353600825)) ;
#13888 = CARTESIAN_POINT('',(-1.31990818206448,0.87346157265775,1.42830646399175)) ;
#13889 = CARTESIAN_POINT('Origin',(-1.32322330470336,0.876776695296637,1.40375)) ;
#13890 = CARTESIAN_POINT('Origin',(-1.32322330470336,0.876776695296637,1.40375)) ;
#13891 = CARTESIAN_POINT('Origin',(-1.25,0.7,1.37)) ;
#13892 = CARTESIAN_POINT('',(-1.25,0.704688291396844,1.34544353600825)) ;
#13893 = CARTESIAN_POINT('',(-1.25,0.695311708603156,1.39455646399175)) ;
#13894 = CARTESIAN_POINT('Origin',(-1.25,0.7,1.37)) ;
#13895 = CARTESIAN_POINT('Origin',(-1.25,0.7,1.37)) ;
#13896 = CARTESIAN_POINT('Origin',(-1.32322330470336,0.523223304703363,1.33625)) ;
#13897 = CARTESIAN_POINT('',(-1.31990818206448,0.52653842734225,1.31169353600825)) ;
#13898 = CARTESIAN_POINT('',(-1.32653842734225,0.519908182064476,1.36080646399175)) ;
#13899 = CARTESIAN_POINT('Origin',(-1.32322330470336,0.523223304703363,1.33625)) ;
#13900 = CARTESIAN_POINT('Origin',(-1.32322330470336,0.523223304703363,1.33625)) ;
#13901 = CARTESIAN_POINT('Origin',(-1.5,0.45,1.3025)) ;
#13902 = CARTESIAN_POINT('',(-1.49531170860316,0.45,1.27794353600825)) ;
#13903 = CARTESIAN_POINT('',(-1.50468829139684,0.45,1.32705646399175)) ;
#13904 = CARTESIAN_POINT('Origin',(-1.5,0.45,1.3025)) ;
#13905 = CARTESIAN_POINT('',(-1.51037428027778,0.429342812247576,1.31202128682895)) ;
#13906 = CARTESIAN_POINT('Origin',(-1.5,0.45,1.3025)) ;
#13907 = CARTESIAN_POINT('Origin',(-1.5,0.45,1.3025)) ;
#13908 = CARTESIAN_POINT('Origin',(-1.67677669529664,0.523223304703363,1.26875)) ;
#13909 = CARTESIAN_POINT('',(-1.67346157265775,0.519908182064476,1.24419353600825)) ;
#13910 = CARTESIAN_POINT('',(-1.68715097557442,0.502566116950939,1.27827128682895)) ;
#13911 = CARTESIAN_POINT('Origin',(-1.67677669529664,0.523223304703363,1.26875)) ;
#13912 = CARTESIAN_POINT('',(-1.68009181793552,0.52653842734225,1.29330646399175)) ;
#13913 = CARTESIAN_POINT('Origin',(-1.67677669529664,0.523223304703363,1.26875)) ;
#13914 = CARTESIAN_POINT('',(-1.69993339200128,0.513968813087923,1.27051685671998)) ;
#13915 = CARTESIAN_POINT('Origin',(-1.67677669529664,0.523223304703363,1.26875)) ;
#13916 = CARTESIAN_POINT('Origin',(-1.67677669529664,0.523223304703363,1.26875)) ;
#13917 = CARTESIAN_POINT('Origin',(-1.75,0.7,1.235)) ;
#13918 = CARTESIAN_POINT('',(-1.75,0.695311708603157,1.21044353600825)) ;
#13919 = CARTESIAN_POINT('',(-1.77315669670464,0.69074550838456,1.23676685671998)) ;
#13920 = CARTESIAN_POINT('Origin',(-1.75,0.7,1.235)) ;
#13921 = CARTESIAN_POINT('',(-1.75,0.704688291396844,1.25955646399175)) ;
#13922 = CARTESIAN_POINT('Origin',(-1.75,0.7,1.235)) ;
#13923 = CARTESIAN_POINT('',(-1.77315669670464,0.70925449161544,1.23323314328002)) ;
#13924 = CARTESIAN_POINT('Origin',(-1.75,0.7,1.235)) ;
#13925 = CARTESIAN_POINT('Origin',(-1.75,0.7,1.235)) ;
#13926 = CARTESIAN_POINT('Origin',(-1.67677669529664,0.876776695296637,1.20125)) ;
#13927 = CARTESIAN_POINT('',(-1.68009181793552,0.87346157265775,1.17669353600825)) ;
#13928 = CARTESIAN_POINT('',(-1.69993339200128,0.886031186912078,1.19948314328002)) ;
#13929 = CARTESIAN_POINT('Origin',(-1.67677669529664,0.876776695296637,1.20125)) ;
#13930 = CARTESIAN_POINT('',(-1.67346157265775,0.880091817935524,1.22580646399175)) ;
#13931 = CARTESIAN_POINT('Origin',(-1.67677669529664,0.876776695296637,1.20125)) ;
#13932 = CARTESIAN_POINT('',(-1.68715097557442,0.897433883049061,1.19172871317105)) ;
#13933 = CARTESIAN_POINT('Origin',(-1.67677669529664,0.876776695296637,1.20125)) ;
#13934 = CARTESIAN_POINT('Origin',(-1.67677669529664,0.876776695296637,1.20125)) ;
#13935 = CARTESIAN_POINT('Origin',(-1.5,0.95,1.1675)) ;
#13936 = CARTESIAN_POINT('',(-1.50468829139684,0.95,1.14294353600825)) ;
#13937 = CARTESIAN_POINT('',(-1.51037428027778,0.970657187752424,1.15797871317105)) ;
#13938 = CARTESIAN_POINT('Origin',(-1.5,0.95,1.1675)) ;
#13939 = CARTESIAN_POINT('',(-1.49531170860316,0.95,1.19205646399175)) ;
#13940 = CARTESIAN_POINT('Origin',(-1.5,0.95,1.1675)) ;
#13941 = CARTESIAN_POINT('Origin',(-1.5,0.95,1.1675)) ;
#13942 = CARTESIAN_POINT('Origin',(-1.32322330470336,0.876776695296637,1.13375)) ;
#13943 = CARTESIAN_POINT('',(-1.32653842734225,0.880091817935524,1.10919353600825)) ;
#13944 = CARTESIAN_POINT('',(-1.31990818206448,0.87346157265775,1.15830646399175)) ;
#13945 = CARTESIAN_POINT('Origin',(-1.32322330470336,0.876776695296637,1.13375)) ;
#13946 = CARTESIAN_POINT('Origin',(-1.32322330470336,0.876776695296637,1.13375)) ;
#13947 = CARTESIAN_POINT('Origin',(-1.25,0.7,1.1)) ;
#13948 = CARTESIAN_POINT('',(-1.25,0.704688291396844,1.07544353600825)) ;
#13949 = CARTESIAN_POINT('',(-1.25,0.695311708603156,1.12455646399175)) ;
#13950 = CARTESIAN_POINT('Origin',(-1.25,0.7,1.1)) ;
#13951 = CARTESIAN_POINT('Origin',(-1.25,0.7,1.1)) ;
#13952 = CARTESIAN_POINT('Origin',(-1.32322330470336,0.523223304703363,1.06625)) ;
#13953 = CARTESIAN_POINT('',(-1.31990818206448,0.52653842734225,1.04169353600825)) ;
#13954 = CARTESIAN_POINT('',(-1.32653842734225,0.519908182064476,1.09080646399175)) ;
#13955 = CARTESIAN_POINT('Origin',(-1.32322330470336,0.523223304703363,1.06625)) ;
#13956 = CARTESIAN_POINT('Origin',(-1.32322330470336,0.523223304703363,1.06625)) ;
#13957 = CARTESIAN_POINT('Origin',(-1.5,0.45,1.0325)) ;
#13958 = CARTESIAN_POINT('',(-1.49531170860316,0.45,1.00794353600825)) ;
#13959 = CARTESIAN_POINT('',(-1.50468829139684,0.45,1.05705646399175)) ;
#13960 = CARTESIAN_POINT('Origin',(-1.5,0.45,1.0325)) ;
#13961 = CARTESIAN_POINT('',(-1.51037428027778,0.429342812247576,1.04202128682895)) ;
#13962 = CARTESIAN_POINT('Origin',(-1.5,0.45,1.0325)) ;
#13963 = CARTESIAN_POINT('Origin',(-1.5,0.45,1.0325)) ;
#13964 = CARTESIAN_POINT('Origin',(-1.67677669529664,0.523223304703363,0.99875)) ;
#13965 = CARTESIAN_POINT('',(-1.67346157265775,0.519908182064476,0.974193536008247)) ;
#13966 = CARTESIAN_POINT('',(-1.68715097557442,0.502566116950939,1.00827128682895)) ;
#13967 = CARTESIAN_POINT('Origin',(-1.67677669529664,0.523223304703363,0.99875)) ;
#13968 = CARTESIAN_POINT('',(-1.68009181793552,0.52653842734225,1.02330646399175)) ;
#13969 = CARTESIAN_POINT('Origin',(-1.67677669529664,0.523223304703363,0.99875)) ;
#13970 = CARTESIAN_POINT('',(-1.69993339200128,0.513968813087922,1.00051685671998)) ;
#13971 = CARTESIAN_POINT('Origin',(-1.67677669529664,0.523223304703363,0.99875)) ;
#13972 = CARTESIAN_POINT('Origin',(-1.67677669529664,0.523223304703363,0.99875)) ;
#13973 = CARTESIAN_POINT('Origin',(-1.75,0.7,0.965)) ;
#13974 = CARTESIAN_POINT('',(-1.75,0.695311708603157,0.940443536008247)) ;
#13975 = CARTESIAN_POINT('',(-1.77315669670464,0.69074550838456,0.966766856719982)) ;
#13976 = CARTESIAN_POINT('Origin',(-1.75,0.7,0.965)) ;
#13977 = CARTESIAN_POINT('',(-1.75,0.704688291396844,0.989556463991753)) ;
#13978 = CARTESIAN_POINT('Origin',(-1.75,0.7,0.965)) ;
#13979 = CARTESIAN_POINT('',(-1.77315669670464,0.709254491615441,0.963233143280018)) ;
#13980 = CARTESIAN_POINT('Origin',(-1.75,0.7,0.965)) ;
#13981 = CARTESIAN_POINT('Origin',(-1.75,0.7,0.965)) ;
#13982 = CARTESIAN_POINT('Origin',(-1.67677669529664,0.876776695296637,0.93125)) ;
#13983 = CARTESIAN_POINT('',(-1.68009181793552,0.87346157265775,0.906693536008247)) ;
#13984 = CARTESIAN_POINT('',(-1.69993339200128,0.886031186912078,0.929483143280018)) ;
#13985 = CARTESIAN_POINT('Origin',(-1.67677669529664,0.876776695296637,0.93125)) ;
#13986 = CARTESIAN_POINT('',(-1.67346157265775,0.880091817935524,0.955806463991753)) ;
#13987 = CARTESIAN_POINT('Origin',(-1.67677669529664,0.876776695296637,0.93125)) ;
#13988 = CARTESIAN_POINT('',(-1.68715097557442,0.897433883049061,0.92172871317105)) ;
#13989 = CARTESIAN_POINT('Origin',(-1.67677669529664,0.876776695296637,0.93125)) ;
#13990 = CARTESIAN_POINT('Origin',(-1.67677669529664,0.876776695296637,0.93125)) ;
#13991 = CARTESIAN_POINT('Origin',(-1.5,0.95,0.8975)) ;
#13992 = CARTESIAN_POINT('',(-1.50468829139684,0.95,0.872943536008246)) ;
#13993 = CARTESIAN_POINT('',(-1.51037428027778,0.970657187752424,0.88797871317105)) ;
#13994 = CARTESIAN_POINT('Origin',(-1.5,0.95,0.8975)) ;
#13995 = CARTESIAN_POINT('',(-1.49531170860316,0.950000000000001,0.922056463991753)) ;
#13996 = CARTESIAN_POINT('Origin',(-1.5,0.95,0.8975)) ;
#13997 = CARTESIAN_POINT('Origin',(-1.5,0.95,0.8975)) ;
#13998 = CARTESIAN_POINT('Origin',(-1.32322330470336,0.876776695296637,0.86375)) ;
#13999 = CARTESIAN_POINT('',(-1.32653842734225,0.880091817935523,0.839193536008247)) ;
#14000 = CARTESIAN_POINT('',(-1.31990818206448,0.87346157265775,0.888306463991753)) ;
#14001 = CARTESIAN_POINT('Origin',(-1.32322330470336,0.876776695296637,0.86375)) ;
#14002 = CARTESIAN_POINT('Origin',(-1.32322330470336,0.876776695296637,0.86375)) ;
#14003 = CARTESIAN_POINT('Origin',(-1.25,0.7,0.83)) ;
#14004 = CARTESIAN_POINT('',(-1.25,0.704688291396844,0.805443536008247)) ;
#14005 = CARTESIAN_POINT('',(-1.25,0.695311708603156,0.854556463991753)) ;
#14006 = CARTESIAN_POINT('Origin',(-1.25,0.7,0.83)) ;
#14007 = CARTESIAN_POINT('Origin',(-1.25,0.7,0.83)) ;
#14008 = CARTESIAN_POINT('Origin',(-1.32322330470336,0.523223304703363,0.79625)) ;
#14009 = CARTESIAN_POINT('',(-1.31990818206448,0.52653842734225,0.771693536008247)) ;
#14010 = CARTESIAN_POINT('',(-1.32653842734225,0.519908182064476,0.820806463991753)) ;
#14011 = CARTESIAN_POINT('Origin',(-1.32322330470336,0.523223304703363,0.79625)) ;
#14012 = CARTESIAN_POINT('Origin',(-1.32322330470336,0.523223304703363,0.79625)) ;
#14013 = CARTESIAN_POINT('Origin',(-1.5,0.45,0.7625)) ;
#14014 = CARTESIAN_POINT('',(-1.49531170860316,0.45,0.737943536008247)) ;
#14015 = CARTESIAN_POINT('',(-1.50468829139684,0.45,0.787056463991754)) ;
#14016 = CARTESIAN_POINT('Origin',(-1.5,0.45,0.7625)) ;
#14017 = CARTESIAN_POINT('',(-1.51037428027778,0.429342812247576,0.77202128682895)) ;
#14018 = CARTESIAN_POINT('Origin',(-1.5,0.45,0.7625)) ;
#14019 = CARTESIAN_POINT('Origin',(-1.5,0.45,0.7625)) ;
#14020 = CARTESIAN_POINT('Origin',(-1.67677669529664,0.523223304703363,0.72875)) ;
#14021 = CARTESIAN_POINT('',(-1.67346157265775,0.519908182064476,0.704193536008247)) ;
#14022 = CARTESIAN_POINT('',(-1.68715097557442,0.502566116950939,0.73827128682895)) ;
#14023 = CARTESIAN_POINT('Origin',(-1.67677669529664,0.523223304703363,0.72875)) ;
#14024 = CARTESIAN_POINT('',(-1.68009181793552,0.52653842734225,0.753306463991753)) ;
#14025 = CARTESIAN_POINT('Origin',(-1.67677669529664,0.523223304703363,0.72875)) ;
#14026 = CARTESIAN_POINT('',(-1.69993339200128,0.513968813087923,0.730516856719982)) ;
#14027 = CARTESIAN_POINT('Origin',(-1.67677669529664,0.523223304703363,0.72875)) ;
#14028 = CARTESIAN_POINT('Origin',(-1.67677669529664,0.523223304703363,0.72875)) ;
#14029 = CARTESIAN_POINT('Origin',(-1.75,0.7,0.695)) ;
#14030 = CARTESIAN_POINT('',(-1.75,0.695311708603156,0.670443536008247)) ;
#14031 = CARTESIAN_POINT('',(-1.77315669670464,0.69074550838456,0.696766856719982)) ;
#14032 = CARTESIAN_POINT('Origin',(-1.75,0.7,0.695)) ;
#14033 = CARTESIAN_POINT('',(-1.75,0.704688291396844,0.719556463991753)) ;
#14034 = CARTESIAN_POINT('Origin',(-1.75,0.7,0.695)) ;
#14035 = CARTESIAN_POINT('',(-1.77315669670464,0.70925449161544,0.693233143280018)) ;
#14036 = CARTESIAN_POINT('Origin',(-1.75,0.7,0.695)) ;
#14037 = CARTESIAN_POINT('Origin',(-1.75,0.7,0.695)) ;
#14038 = CARTESIAN_POINT('Origin',(-1.67677669529664,0.876776695296637,0.66125)) ;
#14039 = CARTESIAN_POINT('',(-1.68009181793552,0.87346157265775,0.636693536008247)) ;
#14040 = CARTESIAN_POINT('',(-1.69993339200128,0.886031186912077,0.659483143280018)) ;
#14041 = CARTESIAN_POINT('Origin',(-1.67677669529664,0.876776695296637,0.66125)) ;
#14042 = CARTESIAN_POINT('',(-1.67346157265775,0.880091817935524,0.685806463991753)) ;
#14043 = CARTESIAN_POINT('Origin',(-1.67677669529664,0.876776695296637,0.66125)) ;
#14044 = CARTESIAN_POINT('',(-1.68715097557442,0.897433883049061,0.65172871317105)) ;
#14045 = CARTESIAN_POINT('Origin',(-1.67677669529664,0.876776695296637,0.66125)) ;
#14046 = CARTESIAN_POINT('Origin',(-1.67677669529664,0.876776695296637,0.66125)) ;
#14047 = CARTESIAN_POINT('Origin',(-1.5,0.95,0.6275)) ;
#14048 = CARTESIAN_POINT('',(-1.50468829139684,0.95,0.602943536008246)) ;
#14049 = CARTESIAN_POINT('',(-1.51037428027778,0.970657187752424,0.61797871317105)) ;
#14050 = CARTESIAN_POINT('Origin',(-1.5,0.95,0.6275)) ;
#14051 = CARTESIAN_POINT('',(-1.49531170860316,0.95,0.652056463991753)) ;
#14052 = CARTESIAN_POINT('Origin',(-1.5,0.95,0.6275)) ;
#14053 = CARTESIAN_POINT('Origin',(-1.5,0.95,0.6275)) ;
#14054 = CARTESIAN_POINT('Origin',(-1.32322330470336,0.876776695296637,0.59375)) ;
#14055 = CARTESIAN_POINT('',(-1.32653842734225,0.880091817935524,0.569193536008247)) ;
#14056 = CARTESIAN_POINT('',(-1.31990818206448,0.87346157265775,0.618306463991753)) ;
#14057 = CARTESIAN_POINT('Origin',(-1.32322330470336,0.876776695296637,0.59375)) ;
#14058 = CARTESIAN_POINT('Origin',(-1.32322330470336,0.876776695296637,0.59375)) ;
#14059 = CARTESIAN_POINT('Origin',(-1.28661165235168,0.611611652351681,1.893125)) ;
#14060 = CARTESIAN_POINT('',(-1.27315669670464,0.70925449161544,1.91176685671998)) ;
#14061 = CARTESIAN_POINT('Origin',(-1.25,0.7,1.91)) ;
#14062 = CARTESIAN_POINT('',(-1.34258615076189,0.541636962002279,1.87976551392448)) ;
#14063 = CARTESIAN_POINT('',(-1.30976834905632,0.620866143967122,1.89489185671998)) ;
#14064 = CARTESIAN_POINT('',(-1.34236685176283,0.540248143222746,1.88409706866696)) ;
#14065 = CARTESIAN_POINT('Origin',(-1.32322330470336,0.523223304703363,1.87625)) ;
#14066 = CARTESIAN_POINT('Origin',(-1.32322330470336,0.523223304703363,1.87625)) ;
#14067 = CARTESIAN_POINT('Origin',(-1.32322330470336,0.523223304703363,1.87625)) ;
#14068 = CARTESIAN_POINT('Origin',(-1.25,0.7,1.91)) ;
#14069 = CARTESIAN_POINT('Origin',(-1.41161165235168,0.486611652351681,1.859375)) ;
#14070 = CARTESIAN_POINT('',(-1.50211870854008,0.474076757531324,1.85359743093369)) ;
#14071 = CARTESIAN_POINT('',(-1.42198593262946,0.507268840104105,1.86889628682895)) ;
#14072 = CARTESIAN_POINT('Origin',(-1.5,0.45,1.8425)) ;
#14073 = CARTESIAN_POINT('Origin',(-1.5,0.45,1.8425)) ;
#14074 = CARTESIAN_POINT('Origin',(-1.58838834764832,0.486611652351682,1.825625)) ;
#14075 = CARTESIAN_POINT('',(-1.5987626279261,0.465954464599258,1.83514628682895)) ;
#14076 = CARTESIAN_POINT('Origin',(-1.67677669529664,0.523223304703363,1.80875)) ;
#14077 = CARTESIAN_POINT('Origin',(-1.71338834764832,0.611611652351682,1.791875)) ;
#14078 = CARTESIAN_POINT('',(-1.73654504435296,0.602357160736241,1.79364185671998)) ;
#14079 = CARTESIAN_POINT('Origin',(-1.75,0.7,1.775)) ;
#14080 = CARTESIAN_POINT('Origin',(-1.71338834764832,0.788388347648319,1.758125)) ;
#14081 = CARTESIAN_POINT('',(-1.73654504435296,0.797642839263759,1.75635814328002)) ;
#14082 = CARTESIAN_POINT('Origin',(-1.67677669529664,0.876776695296637,1.74125)) ;
#14083 = CARTESIAN_POINT('Origin',(-1.58838834764832,0.913388347648319,1.724375)) ;
#14084 = CARTESIAN_POINT('',(-1.5987626279261,0.934045535400743,1.71485371317105)) ;
#14085 = CARTESIAN_POINT('',(-1.50211870854008,0.925923242468676,1.69640256906631)) ;
#14086 = CARTESIAN_POINT('Origin',(-1.5,0.95,1.7075)) ;
#14087 = CARTESIAN_POINT('Origin',(-1.5,0.95,1.7075)) ;
#14088 = CARTESIAN_POINT('Origin',(-1.41161165235168,0.913388347648318,1.690625)) ;
#14089 = CARTESIAN_POINT('',(-1.34236685176283,0.859751856777253,1.66590293133304)) ;
#14090 = CARTESIAN_POINT('',(-1.42198593262946,0.892731159895895,1.68110371317105)) ;
#14091 = CARTESIAN_POINT('',(-1.34258615076189,0.858363037997721,1.67023448607552)) ;
#14092 = CARTESIAN_POINT('Origin',(-1.32322330470336,0.876776695296637,1.67375)) ;
#14093 = CARTESIAN_POINT('Origin',(-1.32322330470336,0.876776695296637,1.67375)) ;
#14094 = CARTESIAN_POINT('Origin',(-1.32322330470336,0.876776695296637,1.67375)) ;
#14095 = CARTESIAN_POINT('Origin',(-1.28661165235168,0.788388347648318,1.656875)) ;
#14096 = CARTESIAN_POINT('',(-1.27699003264463,0.7,1.64)) ;
#14097 = CARTESIAN_POINT('',(-1.30976834905632,0.779133856032878,1.65510814328002)) ;
#14098 = CARTESIAN_POINT('Origin',(-1.25,0.7,1.64)) ;
#14099 = CARTESIAN_POINT('Origin',(-1.25,0.7,1.64)) ;
#14100 = CARTESIAN_POINT('Origin',(-1.28661165235168,0.611611652351681,1.623125)) ;
#14101 = CARTESIAN_POINT('',(-1.34258615076189,0.541636962002279,1.60976551392448)) ;
#14102 = CARTESIAN_POINT('',(-1.30976834905632,0.620866143967122,1.62489185671998)) ;
#14103 = CARTESIAN_POINT('',(-1.34236685176283,0.540248143222746,1.61409706866696)) ;
#14104 = CARTESIAN_POINT('Origin',(-1.32322330470336,0.523223304703363,1.60625)) ;
#14105 = CARTESIAN_POINT('Origin',(-1.32322330470336,0.523223304703363,1.60625)) ;
#14106 = CARTESIAN_POINT('Origin',(-1.32322330470336,0.523223304703363,1.60625)) ;
#14107 = CARTESIAN_POINT('Origin',(-1.41161165235168,0.486611652351681,1.589375)) ;
#14108 = CARTESIAN_POINT('',(-1.50211870854008,0.474076757531324,1.58359743093369)) ;
#14109 = CARTESIAN_POINT('',(-1.42198593262946,0.507268840104105,1.59889628682895)) ;
#14110 = CARTESIAN_POINT('Origin',(-1.5,0.45,1.5725)) ;
#14111 = CARTESIAN_POINT('Origin',(-1.5,0.45,1.5725)) ;
#14112 = CARTESIAN_POINT('Origin',(-1.58838834764832,0.486611652351682,1.555625)) ;
#14113 = CARTESIAN_POINT('',(-1.5987626279261,0.465954464599258,1.56514628682895)) ;
#14114 = CARTESIAN_POINT('Origin',(-1.67677669529664,0.523223304703363,1.53875)) ;
#14115 = CARTESIAN_POINT('Origin',(-1.71338834764832,0.611611652351682,1.521875)) ;
#14116 = CARTESIAN_POINT('',(-1.73654504435296,0.602357160736241,1.52364185671998)) ;
#14117 = CARTESIAN_POINT('Origin',(-1.75,0.7,1.505)) ;
#14118 = CARTESIAN_POINT('Origin',(-1.71338834764832,0.788388347648319,1.488125)) ;
#14119 = CARTESIAN_POINT('',(-1.73654504435296,0.797642839263759,1.48635814328002)) ;
#14120 = CARTESIAN_POINT('Origin',(-1.67677669529664,0.876776695296637,1.47125)) ;
#14121 = CARTESIAN_POINT('Origin',(-1.58838834764832,0.913388347648319,1.454375)) ;
#14122 = CARTESIAN_POINT('',(-1.5987626279261,0.934045535400743,1.44485371317105)) ;
#14123 = CARTESIAN_POINT('',(-1.50211870854008,0.925923242468676,1.42640256906631)) ;
#14124 = CARTESIAN_POINT('Origin',(-1.5,0.95,1.4375)) ;
#14125 = CARTESIAN_POINT('Origin',(-1.5,0.95,1.4375)) ;
#14126 = CARTESIAN_POINT('Origin',(-1.41161165235168,0.913388347648318,1.420625)) ;
#14127 = CARTESIAN_POINT('',(-1.34236685176283,0.859751856777253,1.39590293133304)) ;
#14128 = CARTESIAN_POINT('',(-1.42198593262946,0.892731159895895,1.41110371317105)) ;
#14129 = CARTESIAN_POINT('',(-1.34258615076189,0.858363037997721,1.40023448607552)) ;
#14130 = CARTESIAN_POINT('Origin',(-1.32322330470336,0.876776695296637,1.40375)) ;
#14131 = CARTESIAN_POINT('Origin',(-1.32322330470336,0.876776695296637,1.40375)) ;
#14132 = CARTESIAN_POINT('Origin',(-1.32322330470336,0.876776695296637,1.40375)) ;
#14133 = CARTESIAN_POINT('Origin',(-1.28661165235168,0.788388347648318,1.386875)) ;
#14134 = CARTESIAN_POINT('',(-1.27699003264463,0.7,1.37)) ;
#14135 = CARTESIAN_POINT('',(-1.30976834905632,0.779133856032878,1.38510814328002)) ;
#14136 = CARTESIAN_POINT('Origin',(-1.25,0.7,1.37)) ;
#14137 = CARTESIAN_POINT('Origin',(-1.25,0.7,1.37)) ;
#14138 = CARTESIAN_POINT('Origin',(-1.28661165235168,0.611611652351681,1.353125)) ;
#14139 = CARTESIAN_POINT('',(-1.34258615076189,0.541636962002279,1.33976551392448)) ;
#14140 = CARTESIAN_POINT('',(-1.30976834905632,0.620866143967122,1.35489185671998)) ;
#14141 = CARTESIAN_POINT('',(-1.34236685176283,0.540248143222746,1.34409706866696)) ;
#14142 = CARTESIAN_POINT('Origin',(-1.32322330470336,0.523223304703363,1.33625)) ;
#14143 = CARTESIAN_POINT('Origin',(-1.32322330470336,0.523223304703363,1.33625)) ;
#14144 = CARTESIAN_POINT('Origin',(-1.32322330470336,0.523223304703363,1.33625)) ;
#14145 = CARTESIAN_POINT('Origin',(-1.41161165235168,0.486611652351681,1.319375)) ;
#14146 = CARTESIAN_POINT('',(-1.50211870854008,0.474076757531324,1.31359743093369)) ;
#14147 = CARTESIAN_POINT('',(-1.42198593262946,0.507268840104105,1.32889628682895)) ;
#14148 = CARTESIAN_POINT('Origin',(-1.5,0.45,1.3025)) ;
#14149 = CARTESIAN_POINT('Origin',(-1.5,0.45,1.3025)) ;
#14150 = CARTESIAN_POINT('Origin',(-1.58838834764832,0.486611652351682,1.285625)) ;
#14151 = CARTESIAN_POINT('',(-1.5987626279261,0.465954464599258,1.29514628682895)) ;
#14152 = CARTESIAN_POINT('Origin',(-1.67677669529664,0.523223304703363,1.26875)) ;
#14153 = CARTESIAN_POINT('Origin',(-1.71338834764832,0.611611652351682,1.251875)) ;
#14154 = CARTESIAN_POINT('',(-1.73654504435296,0.602357160736241,1.25364185671998)) ;
#14155 = CARTESIAN_POINT('Origin',(-1.75,0.7,1.235)) ;
#14156 = CARTESIAN_POINT('Origin',(-1.71338834764832,0.788388347648319,1.218125)) ;
#14157 = CARTESIAN_POINT('',(-1.73654504435296,0.797642839263759,1.21635814328002)) ;
#14158 = CARTESIAN_POINT('Origin',(-1.67677669529664,0.876776695296637,1.20125)) ;
#14159 = CARTESIAN_POINT('Origin',(-1.58838834764832,0.913388347648319,1.184375)) ;
#14160 = CARTESIAN_POINT('',(-1.5987626279261,0.934045535400743,1.17485371317105)) ;
#14161 = CARTESIAN_POINT('',(-1.50211870854008,0.925923242468676,1.15640256906631)) ;
#14162 = CARTESIAN_POINT('Origin',(-1.5,0.95,1.1675)) ;
#14163 = CARTESIAN_POINT('Origin',(-1.5,0.95,1.1675)) ;
#14164 = CARTESIAN_POINT('Origin',(-1.41161165235168,0.913388347648318,1.150625)) ;
#14165 = CARTESIAN_POINT('',(-1.34236685176283,0.859751856777253,1.12590293133304)) ;
#14166 = CARTESIAN_POINT('',(-1.42198593262946,0.892731159895895,1.14110371317105)) ;
#14167 = CARTESIAN_POINT('',(-1.34258615076189,0.858363037997721,1.13023448607552)) ;
#14168 = CARTESIAN_POINT('Origin',(-1.32322330470336,0.876776695296637,1.13375)) ;
#14169 = CARTESIAN_POINT('Origin',(-1.32322330470336,0.876776695296637,1.13375)) ;
#14170 = CARTESIAN_POINT('Origin',(-1.32322330470336,0.876776695296637,1.13375)) ;
#14171 = CARTESIAN_POINT('Origin',(-1.28661165235168,0.788388347648318,1.116875)) ;
#14172 = CARTESIAN_POINT('',(-1.27699003264463,0.7,1.1)) ;
#14173 = CARTESIAN_POINT('',(-1.30976834905632,0.779133856032878,1.11510814328002)) ;
#14174 = CARTESIAN_POINT('Origin',(-1.25,0.7,1.1)) ;
#14175 = CARTESIAN_POINT('Origin',(-1.25,0.7,1.1)) ;
#14176 = CARTESIAN_POINT('Origin',(-1.28661165235168,0.611611652351681,1.083125)) ;
#14177 = CARTESIAN_POINT('',(-1.34258615076189,0.541636962002279,1.06976551392448)) ;
#14178 = CARTESIAN_POINT('',(-1.30976834905632,0.620866143967122,1.08489185671998)) ;
#14179 = CARTESIAN_POINT('',(-1.34236685176283,0.540248143222746,1.07409706866696)) ;
#14180 = CARTESIAN_POINT('Origin',(-1.32322330470336,0.523223304703363,1.06625)) ;
#14181 = CARTESIAN_POINT('Origin',(-1.32322330470336,0.523223304703363,1.06625)) ;
#14182 = CARTESIAN_POINT('Origin',(-1.32322330470336,0.523223304703363,1.06625)) ;
#14183 = CARTESIAN_POINT('Origin',(-1.41161165235168,0.486611652351681,1.049375)) ;
#14184 = CARTESIAN_POINT('',(-1.50211870854008,0.474076757531324,1.04359743093369)) ;
#14185 = CARTESIAN_POINT('',(-1.42198593262946,0.507268840104105,1.05889628682895)) ;
#14186 = CARTESIAN_POINT('Origin',(-1.5,0.45,1.0325)) ;
#14187 = CARTESIAN_POINT('Origin',(-1.5,0.45,1.0325)) ;
#14188 = CARTESIAN_POINT('Origin',(-1.58838834764832,0.486611652351682,1.015625)) ;
#14189 = CARTESIAN_POINT('',(-1.5987626279261,0.465954464599258,1.02514628682895)) ;
#14190 = CARTESIAN_POINT('Origin',(-1.67677669529664,0.523223304703363,0.99875)) ;
#14191 = CARTESIAN_POINT('Origin',(-1.71338834764832,0.611611652351682,0.981875)) ;
#14192 = CARTESIAN_POINT('',(-1.73654504435296,0.602357160736241,0.983641856719982)) ;
#14193 = CARTESIAN_POINT('Origin',(-1.75,0.7,0.965)) ;
#14194 = CARTESIAN_POINT('Origin',(-1.71338834764832,0.788388347648319,0.948125)) ;
#14195 = CARTESIAN_POINT('',(-1.73654504435296,0.797642839263759,0.946358143280018)) ;
#14196 = CARTESIAN_POINT('Origin',(-1.67677669529664,0.876776695296637,0.93125)) ;
#14197 = CARTESIAN_POINT('Origin',(-1.58838834764832,0.913388347648319,0.914375)) ;
#14198 = CARTESIAN_POINT('',(-1.5987626279261,0.934045535400743,0.90485371317105)) ;
#14199 = CARTESIAN_POINT('',(-1.50211870854008,0.925923242468676,0.886402569066309)) ;
#14200 = CARTESIAN_POINT('Origin',(-1.5,0.95,0.8975)) ;
#14201 = CARTESIAN_POINT('Origin',(-1.5,0.95,0.8975)) ;
#14202 = CARTESIAN_POINT('Origin',(-1.41161165235168,0.913388347648318,0.880625)) ;
#14203 = CARTESIAN_POINT('',(-1.34236685176283,0.859751856777253,0.855902931333038)) ;
#14204 = CARTESIAN_POINT('',(-1.42198593262946,0.892731159895895,0.87110371317105)) ;
#14205 = CARTESIAN_POINT('',(-1.34258615076189,0.858363037997721,0.860234486075523)) ;
#14206 = CARTESIAN_POINT('Origin',(-1.32322330470336,0.876776695296637,0.86375)) ;
#14207 = CARTESIAN_POINT('Origin',(-1.32322330470336,0.876776695296637,0.86375)) ;
#14208 = CARTESIAN_POINT('Origin',(-1.32322330470336,0.876776695296637,0.86375)) ;
#14209 = CARTESIAN_POINT('Origin',(-1.28661165235168,0.788388347648318,0.846875)) ;
#14210 = CARTESIAN_POINT('',(-1.27699003264463,0.7,0.83)) ;
#14211 = CARTESIAN_POINT('',(-1.30976834905632,0.779133856032878,0.845108143280018)) ;
#14212 = CARTESIAN_POINT('Origin',(-1.25,0.7,0.83)) ;
#14213 = CARTESIAN_POINT('Origin',(-1.25,0.7,0.83)) ;
#14214 = CARTESIAN_POINT('Origin',(-1.28661165235168,0.611611652351681,0.813125)) ;
#14215 = CARTESIAN_POINT('',(-1.34258615076189,0.541636962002279,0.799765513924477)) ;
#14216 = CARTESIAN_POINT('',(-1.30976834905632,0.620866143967122,0.814891856719982)) ;
#14217 = CARTESIAN_POINT('',(-1.34236685176283,0.540248143222747,0.804097068666963)) ;
#14218 = CARTESIAN_POINT('Origin',(-1.32322330470336,0.523223304703363,0.79625)) ;
#14219 = CARTESIAN_POINT('Origin',(-1.32322330470336,0.523223304703363,0.79625)) ;
#14220 = CARTESIAN_POINT('Origin',(-1.32322330470336,0.523223304703363,0.79625)) ;
#14221 = CARTESIAN_POINT('Origin',(-1.41161165235168,0.486611652351682,0.779375)) ;
#14222 = CARTESIAN_POINT('',(-1.50211870854008,0.474076757531324,0.773597430933691)) ;
#14223 = CARTESIAN_POINT('',(-1.42198593262946,0.507268840104105,0.78889628682895)) ;
#14224 = CARTESIAN_POINT('Origin',(-1.5,0.45,0.7625)) ;
#14225 = CARTESIAN_POINT('Origin',(-1.5,0.45,0.7625)) ;
#14226 = CARTESIAN_POINT('Origin',(-1.58838834764832,0.486611652351682,0.745625)) ;
#14227 = CARTESIAN_POINT('',(-1.5987626279261,0.465954464599258,0.75514628682895)) ;
#14228 = CARTESIAN_POINT('Origin',(-1.67677669529664,0.523223304703363,0.72875)) ;
#14229 = CARTESIAN_POINT('Origin',(-1.71338834764832,0.611611652351682,0.711875)) ;
#14230 = CARTESIAN_POINT('',(-1.73654504435296,0.602357160736241,0.713641856719982)) ;
#14231 = CARTESIAN_POINT('Origin',(-1.75,0.7,0.695)) ;
#14232 = CARTESIAN_POINT('Origin',(-1.71338834764832,0.788388347648318,0.678125)) ;
#14233 = CARTESIAN_POINT('',(-1.73654504435296,0.797642839263759,0.676358143280018)) ;
#14234 = CARTESIAN_POINT('Origin',(-1.67677669529664,0.876776695296637,0.66125)) ;
#14235 = CARTESIAN_POINT('Origin',(-1.58838834764832,0.913388347648318,0.644375)) ;
#14236 = CARTESIAN_POINT('',(-1.5987626279261,0.934045535400742,0.63485371317105)) ;
#14237 = CARTESIAN_POINT('',(-1.50211870854008,0.925923242468676,0.616402569066309)) ;
#14238 = CARTESIAN_POINT('Origin',(-1.5,0.95,0.6275)) ;
#14239 = CARTESIAN_POINT('Origin',(-1.5,0.95,0.6275)) ;
#14240 = CARTESIAN_POINT('Origin',(-1.41161165235168,0.913388347648318,0.610625)) ;
#14241 = CARTESIAN_POINT('',(-1.34236685176283,0.859751856777253,0.585902931333038)) ;
#14242 = CARTESIAN_POINT('',(-1.42198593262946,0.892731159895895,0.60110371317105)) ;
#14243 = CARTESIAN_POINT('',(-1.34258615076189,0.858363037997721,0.590234486075523)) ;
#14244 = CARTESIAN_POINT('Origin',(-1.32322330470336,0.876776695296637,0.59375)) ;
#14245 = CARTESIAN_POINT('Origin',(-1.32322330470336,0.876776695296637,0.59375)) ;
#14246 = CARTESIAN_POINT('Origin',(-1.32322330470336,0.876776695296637,0.59375)) ;
#14247 = CARTESIAN_POINT('Origin',(-1.28661165235168,0.788388347648318,0.576875)) ;
#14248 = CARTESIAN_POINT('',(-1.27315669670464,0.690745508384559,0.558233143280018)) ;
#14249 = CARTESIAN_POINT('',(-1.30976834905632,0.779133856032878,0.575108143280018)) ;
#14250 = CARTESIAN_POINT('Origin',(-1.25,0.7,0.56)) ;
#14251 = CARTESIAN_POINT('Origin',(-1.25,0.7,0.56)) ;
#14252 = CARTESIAN_POINT('',(0.,0.,0.)) ;
#14253 = CARTESIAN_POINT('Origin',(-3.,1.8,1.7)) ;
#14254 = CARTESIAN_POINT('',(-3.35,1.8,1.7)) ;
#14255 = CARTESIAN_POINT('Origin',(-3.,1.8,1.7)) ;
#14256 = CARTESIAN_POINT('',(-3.2,1.8,1.7)) ;
#14257 = CARTESIAN_POINT('Origin',(-3.,1.8,1.7)) ;
#14258 = CARTESIAN_POINT('Origin',(-3.,1.8,1.9)) ;
#14259 = CARTESIAN_POINT('',(-3.35,1.8,1.9)) ;
#14260 = CARTESIAN_POINT('Origin',(-3.,1.8,1.9)) ;
#14261 = CARTESIAN_POINT('',(-3.2,1.8,1.9)) ;
#14262 = CARTESIAN_POINT('Origin',(-3.,1.8,1.9)) ;
#14263 = CARTESIAN_POINT('Origin',(-3.,1.8,1.8)) ;
#14264 = CARTESIAN_POINT('',(-3.35,1.8,1.8)) ;
#14265 = CARTESIAN_POINT('Origin',(-3.,1.8,1.45)) ;
#14266 = CARTESIAN_POINT('',(-3.2,1.8,2.6)) ;
#14267 = CARTESIAN_POINT('Origin',(-3.,1.8,2.6)) ;
#14268 = CARTESIAN_POINT('',(-3.2,1.8,1.45)) ;
#14269 = CARTESIAN_POINT('Origin',(-3.,1.8,1.45)) ;
#14270 = CARTESIAN_POINT('',(-3.2,1.8,0.3)) ;
#14271 = CARTESIAN_POINT('',(-3.2,1.8,1.45)) ;
#14272 = CARTESIAN_POINT('Origin',(-3.,1.8,0.3)) ;
#14273 = CARTESIAN_POINT('Origin',(-3.,1.8,0.3)) ;
#14274 = CARTESIAN_POINT('Origin',(-3.,1.8,2.6)) ;
#14275 = CARTESIAN_POINT('',(0.,0.,0.)) ;
#14276 = CARTESIAN_POINT('Origin',(-3.,1.8,2.86)) ;
#14277 = CARTESIAN_POINT('',(-2.5,1.5,2.86)) ;
#14278 = CARTESIAN_POINT('',(-2.5,2.1,2.86)) ;
#14279 = CARTESIAN_POINT('',(-2.5,1.8,2.86)) ;
#14280 = CARTESIAN_POINT('',(-3.5,2.1,2.86)) ;
#14281 = CARTESIAN_POINT('',(-3.,2.1,2.86)) ;
#14282 = CARTESIAN_POINT('',(-3.5,1.5,2.86)) ;
#14283 = CARTESIAN_POINT('',(-3.5,1.8,2.86)) ;
#14284 = CARTESIAN_POINT('',(-3.,1.5,2.86)) ;
#14285 = CARTESIAN_POINT('Origin',(-3.,1.5,2.83)) ;
#14286 = CARTESIAN_POINT('',(-3.5,1.5,2.8)) ;
#14287 = CARTESIAN_POINT('',(-3.5,1.5,2.83)) ;
#14288 = CARTESIAN_POINT('',(-2.5,1.5,2.8)) ;
#14289 = CARTESIAN_POINT('',(-3.,1.5,2.8)) ;
#14290 = CARTESIAN_POINT('',(-2.5,1.5,2.83)) ;
#14291 = CARTESIAN_POINT('Origin',(-3.5,1.8,2.83)) ;
#14292 = CARTESIAN_POINT('',(-3.5,2.1,2.8)) ;
#14293 = CARTESIAN_POINT('',(-3.5,2.1,2.83)) ;
#14294 = CARTESIAN_POINT('',(-3.5,1.8,2.8)) ;
#14295 = CARTESIAN_POINT('Origin',(-3.,2.1,2.83)) ;
#14296 = CARTESIAN_POINT('',(-2.5,2.1,2.8)) ;
#14297 = CARTESIAN_POINT('',(-2.5,2.1,2.83)) ;
#14298 = CARTESIAN_POINT('',(-3.,2.1,2.8)) ;
#14299 = CARTESIAN_POINT('Origin',(-2.5,1.8,2.83)) ;
#14300 = CARTESIAN_POINT('',(-2.5,1.8,2.8)) ;
#14301 = CARTESIAN_POINT('Origin',(-3.,1.8,2.5)) ;
#14302 = CARTESIAN_POINT('',(-3.21,1.8,2.4)) ;
#14303 = CARTESIAN_POINT('Origin',(-3.,1.8,2.4)) ;
#14304 = CARTESIAN_POINT('',(-3.21,1.8,2.7)) ;
#14305 = CARTESIAN_POINT('',(-3.21,1.8,2.5)) ;
#14306 = CARTESIAN_POINT('Origin',(-3.,1.8,2.7)) ;
#14307 = CARTESIAN_POINT('Origin',(-3.,1.8,2.7)) ;
#14308 = CARTESIAN_POINT('Origin',(-3.,1.8,2.8)) ;
#14309 = CARTESIAN_POINT('',(-2.3,1.3,2.8)) ;
#14310 = CARTESIAN_POINT('',(-2.3,2.3,2.8)) ;
#14311 = CARTESIAN_POINT('',(-2.3,1.8,2.8)) ;
#14312 = CARTESIAN_POINT('',(-3.7,2.3,2.8)) ;
#14313 = CARTESIAN_POINT('',(-3.,2.3,2.8)) ;
#14314 = CARTESIAN_POINT('',(-3.7,1.3,2.8)) ;
#14315 = CARTESIAN_POINT('',(-3.7,1.8,2.8)) ;
#14316 = CARTESIAN_POINT('',(-3.,1.3,2.8)) ;
#14317 = CARTESIAN_POINT('Origin',(-3.,1.8,2.4)) ;
#14318 = CARTESIAN_POINT('',(-2.3,2.3,2.4)) ;
#14319 = CARTESIAN_POINT('',(-2.3,1.3,2.4)) ;
#14320 = CARTESIAN_POINT('',(-2.3,1.8,2.4)) ;
#14321 = CARTESIAN_POINT('',(-3.7,1.3,2.4)) ;
#14322 = CARTESIAN_POINT('',(-3.,1.3,2.4)) ;
#14323 = CARTESIAN_POINT('',(-3.7,2.3,2.4)) ;
#14324 = CARTESIAN_POINT('',(-3.7,1.8,2.4)) ;
#14325 = CARTESIAN_POINT('',(-3.,2.3,2.4)) ;
#14326 = CARTESIAN_POINT('Origin',(-3.,1.3,2.6)) ;
#14327 = CARTESIAN_POINT('',(-3.7,1.3,2.6)) ;
#14328 = CARTESIAN_POINT('',(-2.3,1.3,2.6)) ;
#14329 = CARTESIAN_POINT('Origin',(-3.7,1.8,2.6)) ;
#14330 = CARTESIAN_POINT('',(-3.7,2.3,2.6)) ;
#14331 = CARTESIAN_POINT('Origin',(-3.,2.3,2.6)) ;
#14332 = CARTESIAN_POINT('',(-2.3,2.3,2.6)) ;
#14333 = CARTESIAN_POINT('Origin',(-2.3,1.8,2.6)) ;
#14334 = CARTESIAN_POINT('',(0.,0.,0.)) ;
#14335 = CARTESIAN_POINT('Origin',(-2.78786796564404,1.58786796564404,2.3525)) ;
#14336 = CARTESIAN_POINT('',(-2.78641456950892,1.58932136177915,2.32758463768377)) ;
#14337 = CARTESIAN_POINT('',(-2.78932136177915,1.58641456950892,2.37741536231623)) ;
#14338 = CARTESIAN_POINT('Origin',(-2.78786796564404,1.58786796564404,2.3525)) ;
#14339 = CARTESIAN_POINT('Origin',(-2.78786796564404,1.58786796564404,2.3525)) ;
#14340 = CARTESIAN_POINT('Origin',(-3.,1.5,2.335)) ;
#14341 = CARTESIAN_POINT('',(-2.99794458747422,1.5,2.31008463768377)) ;
#14342 = CARTESIAN_POINT('',(-3.00205541252578,1.5,2.35991536231623)) ;
#14343 = CARTESIAN_POINT('Origin',(-3.,1.5,2.335)) ;
#14344 = CARTESIAN_POINT('',(-3.00972677312074,1.47741340516083,2.33949840174162)) ;
#14345 = CARTESIAN_POINT('Origin',(-3.,1.5,2.335)) ;
#14346 = CARTESIAN_POINT('Origin',(-3.,1.5,2.335)) ;
#14347 = CARTESIAN_POINT('Origin',(-3.21213203435596,1.58786796564404,2.3175)) ;
#14348 = CARTESIAN_POINT('',(-3.21067863822085,1.58641456950892,2.29258463768377)) ;
#14349 = CARTESIAN_POINT('',(-3.22185880747671,1.56528137080487,2.32199840174162)) ;
#14350 = CARTESIAN_POINT('Origin',(-3.21213203435596,1.58786796564404,2.3175)) ;
#14351 = CARTESIAN_POINT('',(-3.21358543049108,1.58932136177915,2.34241536231623)) ;
#14352 = CARTESIAN_POINT('Origin',(-3.21213203435596,1.58786796564404,2.3175)) ;
#14353 = CARTESIAN_POINT('',(-3.23524046317499,1.5783608422783,2.31828429766351)) ;
#14354 = CARTESIAN_POINT('Origin',(-3.21213203435596,1.58786796564404,2.3175)) ;
#14355 = CARTESIAN_POINT('Origin',(-3.21213203435596,1.58786796564404,2.3175)) ;
#14356 = CARTESIAN_POINT('Origin',(-3.3,1.8,2.3)) ;
#14357 = CARTESIAN_POINT('',(-3.3,1.79794458747422,2.27508463768377)) ;
#14358 = CARTESIAN_POINT('',(-3.32310842881902,1.79049287663427,2.30078429766351)) ;
#14359 = CARTESIAN_POINT('Origin',(-3.3,1.8,2.3)) ;
#14360 = CARTESIAN_POINT('',(-3.3,1.80205541252578,2.32491536231623)) ;
#14361 = CARTESIAN_POINT('Origin',(-3.3,1.8,2.3)) ;
#14362 = CARTESIAN_POINT('',(-3.32310842881902,1.80950712336573,2.29921570233649)) ;
#14363 = CARTESIAN_POINT('Origin',(-3.3,1.8,2.3)) ;
#14364 = CARTESIAN_POINT('Origin',(-3.3,1.8,2.3)) ;
#14365 = CARTESIAN_POINT('Origin',(-3.21213203435596,2.01213203435596,2.2825)) ;
#14366 = CARTESIAN_POINT('',(-3.21358543049108,2.01067863822085,2.25758463768377)) ;
#14367 = CARTESIAN_POINT('',(-3.23524046317498,2.0216391577217,2.28171570233649)) ;
#14368 = CARTESIAN_POINT('Origin',(-3.21213203435596,2.01213203435596,2.2825)) ;
#14369 = CARTESIAN_POINT('',(-3.21067863822085,2.01358543049108,2.30741536231623)) ;
#14370 = CARTESIAN_POINT('Origin',(-3.21213203435596,2.01213203435596,2.2825)) ;
#14371 = CARTESIAN_POINT('',(-3.22185880747671,2.03471862919513,2.27800159825838)) ;
#14372 = CARTESIAN_POINT('Origin',(-3.21213203435596,2.01213203435596,2.2825)) ;
#14373 = CARTESIAN_POINT('Origin',(-3.21213203435596,2.01213203435596,2.2825)) ;
#14374 = CARTESIAN_POINT('Origin',(-3.,2.1,2.265)) ;
#14375 = CARTESIAN_POINT('',(-3.00205541252578,2.1,2.24008463768377)) ;
#14376 = CARTESIAN_POINT('',(-3.00972677312074,2.12258659483917,2.26050159825838)) ;
#14377 = CARTESIAN_POINT('Origin',(-3.,2.1,2.265)) ;
#14378 = CARTESIAN_POINT('',(-2.99794458747422,2.1,2.28991536231623)) ;
#14379 = CARTESIAN_POINT('Origin',(-3.,2.1,2.265)) ;
#14380 = CARTESIAN_POINT('Origin',(-3.,2.1,2.265)) ;
#14381 = CARTESIAN_POINT('Origin',(-2.78786796564404,2.01213203435596,2.2475)) ;
#14382 = CARTESIAN_POINT('',(-2.78932136177915,2.01358543049108,2.22258463768377)) ;
#14383 = CARTESIAN_POINT('',(-2.78641456950892,2.01067863822085,2.27241536231623)) ;
#14384 = CARTESIAN_POINT('Origin',(-2.78786796564404,2.01213203435596,2.2475)) ;
#14385 = CARTESIAN_POINT('Origin',(-2.78786796564404,2.01213203435596,2.2475)) ;
#14386 = CARTESIAN_POINT('Origin',(-2.7,1.8,2.23)) ;
#14387 = CARTESIAN_POINT('',(-2.7,1.80205541252578,2.20508463768377)) ;
#14388 = CARTESIAN_POINT('',(-2.7,1.79794458747422,2.25491536231623)) ;
#14389 = CARTESIAN_POINT('Origin',(-2.7,1.8,2.23)) ;
#14390 = CARTESIAN_POINT('Origin',(-2.7,1.8,2.23)) ;
#14391 = CARTESIAN_POINT('Origin',(-2.78786796564404,1.58786796564404,2.2125)) ;
#14392 = CARTESIAN_POINT('',(-2.78641456950892,1.58932136177915,2.18758463768377)) ;
#14393 = CARTESIAN_POINT('',(-2.78932136177915,1.58641456950892,2.23741536231623)) ;
#14394 = CARTESIAN_POINT('Origin',(-2.78786796564404,1.58786796564404,2.2125)) ;
#14395 = CARTESIAN_POINT('Origin',(-2.78786796564404,1.58786796564404,2.2125)) ;
#14396 = CARTESIAN_POINT('Origin',(-3.,1.5,2.195)) ;
#14397 = CARTESIAN_POINT('',(-2.99794458747422,1.5,2.17008463768377)) ;
#14398 = CARTESIAN_POINT('',(-3.00205541252578,1.5,2.21991536231623)) ;
#14399 = CARTESIAN_POINT('Origin',(-3.,1.5,2.195)) ;
#14400 = CARTESIAN_POINT('',(-3.00972677312074,1.47741340516083,2.19949840174162)) ;
#14401 = CARTESIAN_POINT('Origin',(-3.,1.5,2.195)) ;
#14402 = CARTESIAN_POINT('Origin',(-3.,1.5,2.195)) ;
#14403 = CARTESIAN_POINT('Origin',(-3.21213203435596,1.58786796564404,2.1775)) ;
#14404 = CARTESIAN_POINT('',(-3.21067863822085,1.58641456950892,2.15258463768377)) ;
#14405 = CARTESIAN_POINT('',(-3.22185880747671,1.56528137080487,2.18199840174162)) ;
#14406 = CARTESIAN_POINT('Origin',(-3.21213203435596,1.58786796564404,2.1775)) ;
#14407 = CARTESIAN_POINT('',(-3.21358543049108,1.58932136177915,2.20241536231623)) ;
#14408 = CARTESIAN_POINT('Origin',(-3.21213203435596,1.58786796564404,2.1775)) ;
#14409 = CARTESIAN_POINT('',(-3.23524046317499,1.5783608422783,2.17828429766351)) ;
#14410 = CARTESIAN_POINT('Origin',(-3.21213203435596,1.58786796564404,2.1775)) ;
#14411 = CARTESIAN_POINT('Origin',(-3.21213203435596,1.58786796564404,2.1775)) ;
#14412 = CARTESIAN_POINT('Origin',(-3.3,1.8,2.16)) ;
#14413 = CARTESIAN_POINT('',(-3.3,1.79794458747422,2.13508463768377)) ;
#14414 = CARTESIAN_POINT('',(-3.32310842881902,1.79049287663427,2.16078429766351)) ;
#14415 = CARTESIAN_POINT('Origin',(-3.3,1.8,2.16)) ;
#14416 = CARTESIAN_POINT('',(-3.3,1.80205541252578,2.18491536231623)) ;
#14417 = CARTESIAN_POINT('Origin',(-3.3,1.8,2.16)) ;
#14418 = CARTESIAN_POINT('',(-3.32310842881902,1.80950712336573,2.15921570233649)) ;
#14419 = CARTESIAN_POINT('Origin',(-3.3,1.8,2.16)) ;
#14420 = CARTESIAN_POINT('Origin',(-3.3,1.8,2.16)) ;
#14421 = CARTESIAN_POINT('Origin',(-3.21213203435596,2.01213203435596,2.1425)) ;
#14422 = CARTESIAN_POINT('',(-3.21358543049108,2.01067863822085,2.11758463768377)) ;
#14423 = CARTESIAN_POINT('',(-3.23524046317498,2.0216391577217,2.14171570233649)) ;
#14424 = CARTESIAN_POINT('Origin',(-3.21213203435596,2.01213203435596,2.1425)) ;
#14425 = CARTESIAN_POINT('',(-3.21067863822085,2.01358543049108,2.16741536231623)) ;
#14426 = CARTESIAN_POINT('Origin',(-3.21213203435596,2.01213203435596,2.1425)) ;
#14427 = CARTESIAN_POINT('',(-3.22185880747671,2.03471862919513,2.13800159825838)) ;
#14428 = CARTESIAN_POINT('Origin',(-3.21213203435596,2.01213203435596,2.1425)) ;
#14429 = CARTESIAN_POINT('Origin',(-3.21213203435596,2.01213203435596,2.1425)) ;
#14430 = CARTESIAN_POINT('Origin',(-3.,2.1,2.125)) ;
#14431 = CARTESIAN_POINT('',(-3.00205541252578,2.1,2.10008463768377)) ;
#14432 = CARTESIAN_POINT('',(-3.00972677312074,2.12258659483917,2.12050159825838)) ;
#14433 = CARTESIAN_POINT('Origin',(-3.,2.1,2.125)) ;
#14434 = CARTESIAN_POINT('',(-2.99794458747422,2.1,2.14991536231623)) ;
#14435 = CARTESIAN_POINT('Origin',(-3.,2.1,2.125)) ;
#14436 = CARTESIAN_POINT('Origin',(-3.,2.1,2.125)) ;
#14437 = CARTESIAN_POINT('Origin',(-2.78786796564404,2.01213203435596,2.1075)) ;
#14438 = CARTESIAN_POINT('',(-2.78932136177915,2.01358543049108,2.08258463768377)) ;
#14439 = CARTESIAN_POINT('',(-2.78641456950892,2.01067863822085,2.13241536231623)) ;
#14440 = CARTESIAN_POINT('Origin',(-2.78786796564404,2.01213203435596,2.1075)) ;
#14441 = CARTESIAN_POINT('Origin',(-2.78786796564404,2.01213203435596,2.1075)) ;
#14442 = CARTESIAN_POINT('Origin',(-2.7,1.8,2.09)) ;
#14443 = CARTESIAN_POINT('',(-2.7,1.80205541252578,2.06508463768377)) ;
#14444 = CARTESIAN_POINT('',(-2.7,1.79794458747422,2.11491536231623)) ;
#14445 = CARTESIAN_POINT('Origin',(-2.7,1.8,2.09)) ;
#14446 = CARTESIAN_POINT('Origin',(-2.7,1.8,2.09)) ;
#14447 = CARTESIAN_POINT('Origin',(-2.78786796564404,1.58786796564404,2.0725)) ;
#14448 = CARTESIAN_POINT('',(-2.78641456950892,1.58932136177915,2.04758463768377)) ;
#14449 = CARTESIAN_POINT('',(-2.78932136177915,1.58641456950892,2.09741536231623)) ;
#14450 = CARTESIAN_POINT('Origin',(-2.78786796564404,1.58786796564404,2.0725)) ;
#14451 = CARTESIAN_POINT('Origin',(-2.78786796564404,1.58786796564404,2.0725)) ;
#14452 = CARTESIAN_POINT('Origin',(-3.,1.5,2.055)) ;
#14453 = CARTESIAN_POINT('',(-2.99794458747422,1.5,2.03008463768377)) ;
#14454 = CARTESIAN_POINT('',(-3.00205541252578,1.5,2.07991536231623)) ;
#14455 = CARTESIAN_POINT('Origin',(-3.,1.5,2.055)) ;
#14456 = CARTESIAN_POINT('',(-3.00972677312074,1.47741340516083,2.05949840174162)) ;
#14457 = CARTESIAN_POINT('Origin',(-3.,1.5,2.055)) ;
#14458 = CARTESIAN_POINT('Origin',(-3.,1.5,2.055)) ;
#14459 = CARTESIAN_POINT('Origin',(-3.21213203435596,1.58786796564404,2.0375)) ;
#14460 = CARTESIAN_POINT('',(-3.21067863822085,1.58641456950892,2.01258463768377)) ;
#14461 = CARTESIAN_POINT('',(-3.22185880747671,1.56528137080487,2.04199840174162)) ;
#14462 = CARTESIAN_POINT('Origin',(-3.21213203435596,1.58786796564404,2.0375)) ;
#14463 = CARTESIAN_POINT('',(-3.21358543049108,1.58932136177915,2.06241536231623)) ;
#14464 = CARTESIAN_POINT('Origin',(-3.21213203435596,1.58786796564404,2.0375)) ;
#14465 = CARTESIAN_POINT('',(-3.23524046317499,1.5783608422783,2.03828429766351)) ;
#14466 = CARTESIAN_POINT('Origin',(-3.21213203435596,1.58786796564404,2.0375)) ;
#14467 = CARTESIAN_POINT('Origin',(-3.21213203435596,1.58786796564404,2.0375)) ;
#14468 = CARTESIAN_POINT('Origin',(-3.3,1.8,2.02)) ;
#14469 = CARTESIAN_POINT('',(-3.3,1.79794458747422,1.99508463768377)) ;
#14470 = CARTESIAN_POINT('',(-3.32310842881902,1.79049287663427,2.02078429766351)) ;
#14471 = CARTESIAN_POINT('Origin',(-3.3,1.8,2.02)) ;
#14472 = CARTESIAN_POINT('',(-3.3,1.80205541252578,2.04491536231623)) ;
#14473 = CARTESIAN_POINT('Origin',(-3.3,1.8,2.02)) ;
#14474 = CARTESIAN_POINT('',(-3.32310842881902,1.80950712336573,2.01921570233649)) ;
#14475 = CARTESIAN_POINT('Origin',(-3.3,1.8,2.02)) ;
#14476 = CARTESIAN_POINT('Origin',(-3.3,1.8,2.02)) ;
#14477 = CARTESIAN_POINT('Origin',(-3.21213203435596,2.01213203435596,2.0025)) ;
#14478 = CARTESIAN_POINT('',(-3.21358543049108,2.01067863822085,1.97758463768377)) ;
#14479 = CARTESIAN_POINT('',(-3.23524046317499,2.0216391577217,2.00171570233649)) ;
#14480 = CARTESIAN_POINT('Origin',(-3.21213203435596,2.01213203435596,2.0025)) ;
#14481 = CARTESIAN_POINT('',(-3.21067863822085,2.01358543049108,2.02741536231623)) ;
#14482 = CARTESIAN_POINT('Origin',(-3.21213203435596,2.01213203435596,2.0025)) ;
#14483 = CARTESIAN_POINT('',(-3.22185880747671,2.03471862919513,1.99800159825838)) ;
#14484 = CARTESIAN_POINT('Origin',(-3.21213203435596,2.01213203435596,2.0025)) ;
#14485 = CARTESIAN_POINT('Origin',(-3.21213203435596,2.01213203435596,2.0025)) ;
#14486 = CARTESIAN_POINT('Origin',(-3.,2.1,1.985)) ;
#14487 = CARTESIAN_POINT('',(-3.00205541252578,2.1,1.96008463768377)) ;
#14488 = CARTESIAN_POINT('',(-3.00972677312074,2.12258659483917,1.98050159825838)) ;
#14489 = CARTESIAN_POINT('Origin',(-3.,2.1,1.985)) ;
#14490 = CARTESIAN_POINT('',(-2.99794458747422,2.1,2.00991536231623)) ;
#14491 = CARTESIAN_POINT('Origin',(-3.,2.1,1.985)) ;
#14492 = CARTESIAN_POINT('Origin',(-3.,2.1,1.985)) ;
#14493 = CARTESIAN_POINT('Origin',(-2.78786796564404,2.01213203435596,1.9675)) ;
#14494 = CARTESIAN_POINT('',(-2.78932136177915,2.01358543049108,1.94258463768377)) ;
#14495 = CARTESIAN_POINT('',(-2.78641456950892,2.01067863822085,1.99241536231623)) ;
#14496 = CARTESIAN_POINT('Origin',(-2.78786796564404,2.01213203435596,1.9675)) ;
#14497 = CARTESIAN_POINT('Origin',(-2.78786796564404,2.01213203435596,1.9675)) ;
#14498 = CARTESIAN_POINT('Origin',(-2.74393398282202,1.69393398282202,2.36125)) ;
#14499 = CARTESIAN_POINT('',(-2.72310842881902,1.80950712336573,2.37078429766351)) ;
#14500 = CARTESIAN_POINT('Origin',(-2.7,1.8,2.37)) ;
#14501 = CARTESIAN_POINT('',(-2.80704621154481,1.60686338991361,2.35406704255313)) ;
#14502 = CARTESIAN_POINT('',(-2.76704241164104,1.70344110618775,2.36203429766351)) ;
#14503 = CARTESIAN_POINT('',(-2.80699513023089,1.60656079084632,2.35622290901061)) ;
#14504 = CARTESIAN_POINT('Origin',(-2.78786796564404,1.58786796564404,2.3525)) ;
#14505 = CARTESIAN_POINT('Origin',(-2.78786796564404,1.58786796564404,2.3525)) ;
#14506 = CARTESIAN_POINT('Origin',(-2.78786796564404,1.58786796564404,2.3525)) ;
#14507 = CARTESIAN_POINT('Origin',(-2.7,1.8,2.37)) ;
#14508 = CARTESIAN_POINT('Origin',(-2.89393398282202,1.54393398282202,2.34375)) ;
#14509 = CARTESIAN_POINT('',(-3.00043433938457,1.52643564692014,2.34026498841428)) ;
#14510 = CARTESIAN_POINT('',(-2.90366075594276,1.56652057766118,2.34824840174162)) ;
#14511 = CARTESIAN_POINT('Origin',(-3.,1.5,2.335)) ;
#14512 = CARTESIAN_POINT('Origin',(-3.,1.5,2.335)) ;
#14513 = CARTESIAN_POINT('Origin',(-3.10606601717798,1.54393398282202,2.32625)) ;
#14514 = CARTESIAN_POINT('',(-3.11579279029872,1.52134738798285,2.33074840174162)) ;
#14515 = CARTESIAN_POINT('Origin',(-3.21213203435596,1.58786796564404,2.3175)) ;
#14516 = CARTESIAN_POINT('Origin',(-3.25606601717798,1.69393398282202,2.30875)) ;
#14517 = CARTESIAN_POINT('',(-3.279174445997,1.68442685945629,2.30953429766351)) ;
#14518 = CARTESIAN_POINT('Origin',(-3.3,1.8,2.3)) ;
#14519 = CARTESIAN_POINT('Origin',(-3.25606601717798,1.90606601717798,2.29125)) ;
#14520 = CARTESIAN_POINT('',(-3.279174445997,1.91557314054372,2.29046570233649)) ;
#14521 = CARTESIAN_POINT('Origin',(-3.21213203435596,2.01213203435596,2.2825)) ;
#14522 = CARTESIAN_POINT('Origin',(-3.10606601717798,2.05606601717798,2.27375)) ;
#14523 = CARTESIAN_POINT('',(-3.11579279029872,2.07865261201715,2.26925159825838)) ;
#14524 = CARTESIAN_POINT('',(-3.00043433938457,2.07356435307986,2.25973501158572)) ;
#14525 = CARTESIAN_POINT('Origin',(-3.,2.1,2.265)) ;
#14526 = CARTESIAN_POINT('Origin',(-3.,2.1,2.265)) ;
#14527 = CARTESIAN_POINT('Origin',(-2.89393398282202,2.05606601717798,2.25625)) ;
#14528 = CARTESIAN_POINT('',(-2.80699513023089,1.99343920915368,2.24377709098939)) ;
#14529 = CARTESIAN_POINT('',(-2.90366075594276,2.03347942233882,2.25175159825838)) ;
#14530 = CARTESIAN_POINT('',(-2.80704621154481,1.99313661008639,2.24593295744687)) ;
#14531 = CARTESIAN_POINT('Origin',(-2.78786796564404,2.01213203435596,2.2475)) ;
#14532 = CARTESIAN_POINT('Origin',(-2.78786796564404,2.01213203435596,2.2475)) ;
#14533 = CARTESIAN_POINT('Origin',(-2.78786796564404,2.01213203435596,2.2475)) ;
#14534 = CARTESIAN_POINT('Origin',(-2.74393398282202,1.90606601717798,2.23875)) ;
#14535 = CARTESIAN_POINT('',(-2.72704640825626,1.8,2.23)) ;
#14536 = CARTESIAN_POINT('',(-2.76704241164104,1.89655889381225,2.23796570233649)) ;
#14537 = CARTESIAN_POINT('Origin',(-2.7,1.8,2.23)) ;
#14538 = CARTESIAN_POINT('Origin',(-2.7,1.8,2.23)) ;
#14539 = CARTESIAN_POINT('Origin',(-2.74393398282202,1.69393398282202,2.22125)) ;
#14540 = CARTESIAN_POINT('',(-2.80704621154481,1.60686338991361,2.21406704255313)) ;
#14541 = CARTESIAN_POINT('',(-2.76704241164104,1.70344110618775,2.22203429766351)) ;
#14542 = CARTESIAN_POINT('',(-2.80699513023089,1.60656079084632,2.21622290901061)) ;
#14543 = CARTESIAN_POINT('Origin',(-2.78786796564404,1.58786796564404,2.2125)) ;
#14544 = CARTESIAN_POINT('Origin',(-2.78786796564404,1.58786796564404,2.2125)) ;
#14545 = CARTESIAN_POINT('Origin',(-2.78786796564404,1.58786796564404,2.2125)) ;
#14546 = CARTESIAN_POINT('Origin',(-2.89393398282202,1.54393398282202,2.20375)) ;
#14547 = CARTESIAN_POINT('',(-3.00043433938457,1.52643564692014,2.20026498841428)) ;
#14548 = CARTESIAN_POINT('',(-2.90366075594276,1.56652057766118,2.20824840174162)) ;
#14549 = CARTESIAN_POINT('Origin',(-3.,1.5,2.195)) ;
#14550 = CARTESIAN_POINT('Origin',(-3.,1.5,2.195)) ;
#14551 = CARTESIAN_POINT('Origin',(-3.10606601717798,1.54393398282202,2.18625)) ;
#14552 = CARTESIAN_POINT('',(-3.11579279029872,1.52134738798285,2.19074840174162)) ;
#14553 = CARTESIAN_POINT('Origin',(-3.21213203435596,1.58786796564404,2.1775)) ;
#14554 = CARTESIAN_POINT('Origin',(-3.25606601717798,1.69393398282202,2.16875)) ;
#14555 = CARTESIAN_POINT('',(-3.279174445997,1.68442685945629,2.16953429766351)) ;
#14556 = CARTESIAN_POINT('Origin',(-3.3,1.8,2.16)) ;
#14557 = CARTESIAN_POINT('Origin',(-3.25606601717798,1.90606601717798,2.15125)) ;
#14558 = CARTESIAN_POINT('',(-3.279174445997,1.91557314054372,2.15046570233649)) ;
#14559 = CARTESIAN_POINT('Origin',(-3.21213203435596,2.01213203435596,2.1425)) ;
#14560 = CARTESIAN_POINT('Origin',(-3.10606601717798,2.05606601717798,2.13375)) ;
#14561 = CARTESIAN_POINT('',(-3.11579279029872,2.07865261201715,2.12925159825838)) ;
#14562 = CARTESIAN_POINT('',(-3.00043433938457,2.07356435307986,2.11973501158572)) ;
#14563 = CARTESIAN_POINT('Origin',(-3.,2.1,2.125)) ;
#14564 = CARTESIAN_POINT('Origin',(-3.,2.1,2.125)) ;
#14565 = CARTESIAN_POINT('Origin',(-2.89393398282202,2.05606601717798,2.11625)) ;
#14566 = CARTESIAN_POINT('',(-2.80699513023089,1.99343920915368,2.10377709098939)) ;
#14567 = CARTESIAN_POINT('',(-2.90366075594276,2.03347942233882,2.11175159825838)) ;
#14568 = CARTESIAN_POINT('',(-2.80704621154481,1.99313661008639,2.10593295744687)) ;
#14569 = CARTESIAN_POINT('Origin',(-2.78786796564404,2.01213203435596,2.1075)) ;
#14570 = CARTESIAN_POINT('Origin',(-2.78786796564404,2.01213203435596,2.1075)) ;
#14571 = CARTESIAN_POINT('Origin',(-2.78786796564404,2.01213203435596,2.1075)) ;
#14572 = CARTESIAN_POINT('Origin',(-2.74393398282202,1.90606601717798,2.09875)) ;
#14573 = CARTESIAN_POINT('',(-2.72704640825626,1.8,2.09)) ;
#14574 = CARTESIAN_POINT('',(-2.76704241164104,1.89655889381225,2.09796570233649)) ;
#14575 = CARTESIAN_POINT('Origin',(-2.7,1.8,2.09)) ;
#14576 = CARTESIAN_POINT('Origin',(-2.7,1.8,2.09)) ;
#14577 = CARTESIAN_POINT('Origin',(-2.74393398282202,1.69393398282202,2.08125)) ;
#14578 = CARTESIAN_POINT('',(-2.80704621154481,1.60686338991361,2.07406704255313)) ;
#14579 = CARTESIAN_POINT('',(-2.76704241164104,1.70344110618775,2.08203429766351)) ;
#14580 = CARTESIAN_POINT('',(-2.80699513023089,1.60656079084632,2.07622290901061)) ;
#14581 = CARTESIAN_POINT('Origin',(-2.78786796564404,1.58786796564404,2.0725)) ;
#14582 = CARTESIAN_POINT('Origin',(-2.78786796564404,1.58786796564404,2.0725)) ;
#14583 = CARTESIAN_POINT('Origin',(-2.78786796564404,1.58786796564404,2.0725)) ;
#14584 = CARTESIAN_POINT('Origin',(-2.89393398282202,1.54393398282202,2.06375)) ;
#14585 = CARTESIAN_POINT('',(-3.00043433938457,1.52643564692014,2.06026498841428)) ;
#14586 = CARTESIAN_POINT('',(-2.90366075594276,1.56652057766118,2.06824840174162)) ;
#14587 = CARTESIAN_POINT('Origin',(-3.,1.5,2.055)) ;
#14588 = CARTESIAN_POINT('Origin',(-3.,1.5,2.055)) ;
#14589 = CARTESIAN_POINT('Origin',(-3.10606601717798,1.54393398282202,2.04625)) ;
#14590 = CARTESIAN_POINT('',(-3.11579279029872,1.52134738798285,2.05074840174162)) ;
#14591 = CARTESIAN_POINT('Origin',(-3.21213203435596,1.58786796564404,2.0375)) ;
#14592 = CARTESIAN_POINT('Origin',(-3.25606601717798,1.69393398282202,2.02875)) ;
#14593 = CARTESIAN_POINT('',(-3.279174445997,1.68442685945629,2.02953429766351)) ;
#14594 = CARTESIAN_POINT('Origin',(-3.3,1.8,2.02)) ;
#14595 = CARTESIAN_POINT('Origin',(-3.25606601717798,1.90606601717798,2.01125)) ;
#14596 = CARTESIAN_POINT('',(-3.279174445997,1.91557314054371,2.01046570233649)) ;
#14597 = CARTESIAN_POINT('Origin',(-3.21213203435596,2.01213203435596,2.0025)) ;
#14598 = CARTESIAN_POINT('Origin',(-3.10606601717798,2.05606601717798,1.99375)) ;
#14599 = CARTESIAN_POINT('',(-3.11579279029872,2.07865261201715,1.98925159825838)) ;
#14600 = CARTESIAN_POINT('',(-3.00043433938457,2.07356435307986,1.97973501158572)) ;
#14601 = CARTESIAN_POINT('Origin',(-3.,2.1,1.985)) ;
#14602 = CARTESIAN_POINT('Origin',(-3.,2.1,1.985)) ;
#14603 = CARTESIAN_POINT('Origin',(-2.89393398282202,2.05606601717798,1.97625)) ;
#14604 = CARTESIAN_POINT('',(-2.80699513023089,1.99343920915368,1.96377709098939)) ;
#14605 = CARTESIAN_POINT('',(-2.90366075594276,2.03347942233882,1.97175159825838)) ;
#14606 = CARTESIAN_POINT('',(-2.80704621154481,1.99313661008639,1.96593295744687)) ;
#14607 = CARTESIAN_POINT('Origin',(-2.78786796564404,2.01213203435596,1.9675)) ;
#14608 = CARTESIAN_POINT('Origin',(-2.78786796564404,2.01213203435596,1.9675)) ;
#14609 = CARTESIAN_POINT('Origin',(-2.78786796564404,2.01213203435596,1.9675)) ;
#14610 = CARTESIAN_POINT('Origin',(-2.74393398282202,1.90606601717798,1.95875)) ;
#14611 = CARTESIAN_POINT('',(-2.72310842881902,1.79049287663427,1.94921570233649)) ;
#14612 = CARTESIAN_POINT('',(-2.76704241164104,1.89655889381225,1.95796570233649)) ;
#14613 = CARTESIAN_POINT('Origin',(-2.7,1.8,1.95)) ;
#14614 = CARTESIAN_POINT('Origin',(-2.7,1.8,1.95)) ;
#14615 = CARTESIAN_POINT('',(0.,0.,0.)) ;
#14616 = CARTESIAN_POINT('Origin',(-1.1,-1.75,0.875)) ;
#14617 = CARTESIAN_POINT('',(-1.25,-1.75,0.9)) ;
#14618 = CARTESIAN_POINT('Origin',(-1.1,-1.75,0.9)) ;
#14619 = CARTESIAN_POINT('',(-1.25,-1.75,0.85)) ;
#14620 = CARTESIAN_POINT('',(-1.25,-1.75,0.875)) ;
#14621 = CARTESIAN_POINT('Origin',(-1.1,-1.75,0.85)) ;
#14622 = CARTESIAN_POINT('Origin',(-1.1,-1.75,0.9)) ;
#14623 = CARTESIAN_POINT('Origin',(-1.8,-1.75,0.85)) ;
#14624 = CARTESIAN_POINT('',(-0.9,-2.,0.85)) ;
#14625 = CARTESIAN_POINT('',(-0.9,-1.5,0.85)) ;
#14626 = CARTESIAN_POINT('',(-0.9,-1.75,0.85)) ;
#14627 = CARTESIAN_POINT('',(-2.7,-1.5,0.85)) ;
#14628 = CARTESIAN_POINT('',(-1.8,-1.5,0.85)) ;
#14629 = CARTESIAN_POINT('',(-2.7,-2.,0.85)) ;
#14630 = CARTESIAN_POINT('',(-2.7,-1.75,0.85)) ;
#14631 = CARTESIAN_POINT('',(-1.8,-2.,0.85)) ;
#14632 = CARTESIAN_POINT('Origin',(-1.8,-1.75,0.8)) ;
#14633 = CARTESIAN_POINT('',(-0.9,-1.5,0.8)) ;
#14634 = CARTESIAN_POINT('',(-0.9,-2.,0.8)) ;
#14635 = CARTESIAN_POINT('',(-0.9,-1.75,0.8)) ;
#14636 = CARTESIAN_POINT('',(-2.7,-2.,0.8)) ;
#14637 = CARTESIAN_POINT('',(-1.8,-2.,0.8)) ;
#14638 = CARTESIAN_POINT('',(-2.7,-1.5,0.8)) ;
#14639 = CARTESIAN_POINT('',(-2.7,-1.75,0.8)) ;
#14640 = CARTESIAN_POINT('',(-1.8,-1.5,0.8)) ;
#14641 = CARTESIAN_POINT('Origin',(-1.8,-2.,0.825)) ;
#14642 = CARTESIAN_POINT('',(-2.7,-2.,0.825)) ;
#14643 = CARTESIAN_POINT('',(-0.9,-2.,0.825)) ;
#14644 = CARTESIAN_POINT('Origin',(-2.7,-1.75,0.825)) ;
#14645 = CARTESIAN_POINT('',(-2.7,-1.5,0.825)) ;
#14646 = CARTESIAN_POINT('Origin',(-1.8,-1.5,0.825)) ;
#14647 = CARTESIAN_POINT('',(-0.9,-1.5,0.825)) ;
#14648 = CARTESIAN_POINT('Origin',(-0.9,-1.75,0.825)) ;
#14649 = CARTESIAN_POINT('',(0.,0.,0.)) ;
#14650 = CARTESIAN_POINT('Origin',(-2.6,-1.75,0.55)) ;
#14651 = CARTESIAN_POINT('',(-2.75,-1.75,0.8)) ;
#14652 = CARTESIAN_POINT('Origin',(-2.6,-1.75,0.8)) ;
#14653 = CARTESIAN_POINT('',(-2.75,-1.75,0.3)) ;
#14654 = CARTESIAN_POINT('',(-2.75,-1.75,0.55)) ;
#14655 = CARTESIAN_POINT('Origin',(-2.6,-1.75,0.3)) ;
#14656 = CARTESIAN_POINT('Origin',(-2.6,-1.75,0.3)) ;
#14657 = CARTESIAN_POINT('Origin',(-2.6,-1.75,0.8)) ;
#14658 = CARTESIAN_POINT('Origin',(-2.6,-1.75,0.9)) ;
#14659 = CARTESIAN_POINT('',(-2.75,-1.75,0.95)) ;
#14660 = CARTESIAN_POINT('Origin',(-2.6,-1.75,0.95)) ;
#14661 = CARTESIAN_POINT('',(-2.75,-1.75,0.85)) ;
#14662 = CARTESIAN_POINT('',(-2.75,-1.75,0.9)) ;
#14663 = CARTESIAN_POINT('Origin',(-2.6,-1.75,0.85)) ;
#14664 = CARTESIAN_POINT('Origin',(-2.6,-1.75,0.85)) ;
#14665 = CARTESIAN_POINT('Origin',(-2.6,-1.75,0.95)) ;
#14666 = CARTESIAN_POINT('',(0.,0.,0.)) ;
#14667 = CARTESIAN_POINT('Origin',(-1.1,-1.75,0.5)) ;
#14668 = CARTESIAN_POINT('',(-1.25,-1.75,0.7)) ;
#14669 = CARTESIAN_POINT('Origin',(-1.1,-1.75,0.7)) ;
#14670 = CARTESIAN_POINT('',(-1.25,-1.75,0.3)) ;
#14671 = CARTESIAN_POINT('',(-1.25,-1.75,0.5)) ;
#14672 = CARTESIAN_POINT('Origin',(-1.1,-1.75,0.3)) ;
#14673 = CARTESIAN_POINT('Origin',(-1.1,-1.75,0.3)) ;
#14674 = CARTESIAN_POINT('Origin',(-1.1,-1.75,0.7)) ;
#14675 = CARTESIAN_POINT('',(0.,0.,0.)) ;
#14676 = CARTESIAN_POINT('Origin',(-1.1,-1.75,0.725)) ;
#14677 = CARTESIAN_POINT('',(-1.25,-1.75,0.75)) ;
#14678 = CARTESIAN_POINT('Origin',(-1.1,-1.75,0.75)) ;
#14679 = CARTESIAN_POINT('',(-1.25,-1.75,0.7)) ;
#14680 = CARTESIAN_POINT('',(-1.25,-1.75,0.725)) ;
#14681 = CARTESIAN_POINT('Origin',(-1.1,-1.75,0.7)) ;
#14682 = CARTESIAN_POINT('Origin',(-1.1,-1.75,0.7)) ;
#14683 = CARTESIAN_POINT('Origin',(-1.1,-1.75,0.75)) ;
#14684 = CARTESIAN_POINT('',(0.,0.,0.)) ;
#14685 = CARTESIAN_POINT('Origin',(-1.65857864376269,-1.89142135623731,1.19)) ;
#14686 = CARTESIAN_POINT('',(-1.65758113442658,-1.8904238469012,1.17004981327785)) ;
#14687 = CARTESIAN_POINT('',(-1.6595761530988,-1.89241886557342,1.20995018672215)) ;
#14688 = CARTESIAN_POINT('Origin',(-1.65857864376269,-1.89142135623731,1.19)) ;
#14689 = CARTESIAN_POINT('Origin',(-1.65857864376269,-1.89142135623731,1.19)) ;
#14690 = CARTESIAN_POINT('Origin',(-1.8,-1.95,1.18)) ;
#14691 = CARTESIAN_POINT('',(-1.79858930876828,-1.95,1.16004981327785)) ;
#14692 = CARTESIAN_POINT('',(-1.80141069123172,-1.95,1.19995018672215)) ;
#14693 = CARTESIAN_POINT('Origin',(-1.8,-1.95,1.18)) ;
#14694 = CARTESIAN_POINT('',(-1.80774787444261,-1.96817535490137,1.18310272716026)) ;
#14695 = CARTESIAN_POINT('Origin',(-1.8,-1.95,1.18)) ;
#14696 = CARTESIAN_POINT('Origin',(-1.8,-1.95,1.18)) ;
#14697 = CARTESIAN_POINT('Origin',(-1.94142135623731,-1.89142135623731,1.17)) ;
#14698 = CARTESIAN_POINT('',(-1.9404238469012,-1.89241886557342,1.15004981327785)) ;
#14699 = CARTESIAN_POINT('',(-1.94916923067992,-1.90959671113867,1.17310272716026)) ;
#14700 = CARTESIAN_POINT('Origin',(-1.94142135623731,-1.89142135623731,1.17)) ;
#14701 = CARTESIAN_POINT('',(-1.94241886557342,-1.8904238469012,1.18995018672215)) ;
#14702 = CARTESIAN_POINT('Origin',(-1.94142135623731,-1.89142135623731,1.17)) ;
#14703 = CARTESIAN_POINT('',(-1.95990568186281,-1.89903972277005,1.17053869986369)) ;
#14704 = CARTESIAN_POINT('Origin',(-1.94142135623731,-1.89142135623731,1.17)) ;
#14705 = CARTESIAN_POINT('Origin',(-1.94142135623731,-1.89142135623731,1.17)) ;
#14706 = CARTESIAN_POINT('Origin',(-2.,-1.75,1.16)) ;
#14707 = CARTESIAN_POINT('',(-2.,-1.75141069123172,1.14004981327785)) ;
#14708 = CARTESIAN_POINT('',(-2.0184843256255,-1.75761836653274,1.16053869986369)) ;
#14709 = CARTESIAN_POINT('Origin',(-2.,-1.75,1.16)) ;
#14710 = CARTESIAN_POINT('',(-2.,-1.74858930876828,1.17995018672215)) ;
#14711 = CARTESIAN_POINT('Origin',(-2.,-1.75,1.16)) ;
#14712 = CARTESIAN_POINT('',(-2.0184843256255,-1.74238163346726,1.15946130013631)) ;
#14713 = CARTESIAN_POINT('Origin',(-2.,-1.75,1.16)) ;
#14714 = CARTESIAN_POINT('Origin',(-2.,-1.75,1.16)) ;
#14715 = CARTESIAN_POINT('Origin',(-1.94142135623731,-1.60857864376269,1.15)) ;
#14716 = CARTESIAN_POINT('',(-1.94241886557342,-1.6095761530988,1.13004981327785)) ;
#14717 = CARTESIAN_POINT('',(-1.95990568186281,-1.60096027722995,1.14946130013631)) ;
#14718 = CARTESIAN_POINT('Origin',(-1.94142135623731,-1.60857864376269,1.15)) ;
#14719 = CARTESIAN_POINT('',(-1.9404238469012,-1.60758113442658,1.16995018672215)) ;
#14720 = CARTESIAN_POINT('Origin',(-1.94142135623731,-1.60857864376269,1.15)) ;
#14721 = CARTESIAN_POINT('',(-1.94916923067992,-1.59040328886133,1.14689727283974)) ;
#14722 = CARTESIAN_POINT('Origin',(-1.94142135623731,-1.60857864376269,1.15)) ;
#14723 = CARTESIAN_POINT('Origin',(-1.94142135623731,-1.60857864376269,1.15)) ;
#14724 = CARTESIAN_POINT('Origin',(-1.8,-1.55,1.14)) ;
#14725 = CARTESIAN_POINT('',(-1.80141069123172,-1.55,1.12004981327785)) ;
#14726 = CARTESIAN_POINT('',(-1.80774787444261,-1.53182464509864,1.13689727283974)) ;
#14727 = CARTESIAN_POINT('Origin',(-1.8,-1.55,1.14)) ;
#14728 = CARTESIAN_POINT('',(-1.79858930876828,-1.55,1.15995018672215)) ;
#14729 = CARTESIAN_POINT('Origin',(-1.8,-1.55,1.14)) ;
#14730 = CARTESIAN_POINT('Origin',(-1.8,-1.55,1.14)) ;
#14731 = CARTESIAN_POINT('Origin',(-1.65857864376269,-1.60857864376269,1.13)) ;
#14732 = CARTESIAN_POINT('',(-1.6595761530988,-1.60758113442658,1.11004981327785)) ;
#14733 = CARTESIAN_POINT('',(-1.65758113442658,-1.6095761530988,1.14995018672215)) ;
#14734 = CARTESIAN_POINT('Origin',(-1.65857864376269,-1.60857864376269,1.13)) ;
#14735 = CARTESIAN_POINT('Origin',(-1.65857864376269,-1.60857864376269,1.13)) ;
#14736 = CARTESIAN_POINT('Origin',(-1.6,-1.75,1.12)) ;
#14737 = CARTESIAN_POINT('',(-1.6,-1.74858930876828,1.10004981327785)) ;
#14738 = CARTESIAN_POINT('',(-1.6,-1.75141069123172,1.13995018672215)) ;
#14739 = CARTESIAN_POINT('Origin',(-1.6,-1.75,1.12)) ;
#14740 = CARTESIAN_POINT('Origin',(-1.6,-1.75,1.12)) ;
#14741 = CARTESIAN_POINT('Origin',(-1.65857864376269,-1.89142135623731,1.11)) ;
#14742 = CARTESIAN_POINT('',(-1.65758113442658,-1.8904238469012,1.09004981327785)) ;
#14743 = CARTESIAN_POINT('',(-1.6595761530988,-1.89241886557342,1.12995018672215)) ;
#14744 = CARTESIAN_POINT('Origin',(-1.65857864376269,-1.89142135623731,1.11)) ;
#14745 = CARTESIAN_POINT('Origin',(-1.65857864376269,-1.89142135623731,1.11)) ;
#14746 = CARTESIAN_POINT('Origin',(-1.8,-1.95,1.1)) ;
#14747 = CARTESIAN_POINT('',(-1.79858930876828,-1.95,1.08004981327785)) ;
#14748 = CARTESIAN_POINT('',(-1.80141069123172,-1.95,1.11995018672215)) ;
#14749 = CARTESIAN_POINT('Origin',(-1.8,-1.95,1.1)) ;
#14750 = CARTESIAN_POINT('',(-1.80774787444261,-1.96817535490137,1.10310272716026)) ;
#14751 = CARTESIAN_POINT('Origin',(-1.8,-1.95,1.1)) ;
#14752 = CARTESIAN_POINT('Origin',(-1.8,-1.95,1.1)) ;
#14753 = CARTESIAN_POINT('Origin',(-1.94142135623731,-1.89142135623731,1.09)) ;
#14754 = CARTESIAN_POINT('',(-1.9404238469012,-1.89241886557342,1.07004981327785)) ;
#14755 = CARTESIAN_POINT('',(-1.94916923067992,-1.90959671113867,1.09310272716026)) ;
#14756 = CARTESIAN_POINT('Origin',(-1.94142135623731,-1.89142135623731,1.09)) ;
#14757 = CARTESIAN_POINT('',(-1.94241886557342,-1.8904238469012,1.10995018672215)) ;
#14758 = CARTESIAN_POINT('Origin',(-1.94142135623731,-1.89142135623731,1.09)) ;
#14759 = CARTESIAN_POINT('',(-1.95990568186281,-1.89903972277005,1.09053869986369)) ;
#14760 = CARTESIAN_POINT('Origin',(-1.94142135623731,-1.89142135623731,1.09)) ;
#14761 = CARTESIAN_POINT('Origin',(-1.94142135623731,-1.89142135623731,1.09)) ;
#14762 = CARTESIAN_POINT('Origin',(-2.,-1.75,1.08)) ;
#14763 = CARTESIAN_POINT('',(-2.,-1.75141069123172,1.06004981327785)) ;
#14764 = CARTESIAN_POINT('',(-2.0184843256255,-1.75761836653274,1.08053869986369)) ;
#14765 = CARTESIAN_POINT('Origin',(-2.,-1.75,1.08)) ;
#14766 = CARTESIAN_POINT('',(-2.,-1.74858930876828,1.09995018672215)) ;
#14767 = CARTESIAN_POINT('Origin',(-2.,-1.75,1.08)) ;
#14768 = CARTESIAN_POINT('',(-2.0184843256255,-1.74238163346726,1.07946130013631)) ;
#14769 = CARTESIAN_POINT('Origin',(-2.,-1.75,1.08)) ;
#14770 = CARTESIAN_POINT('Origin',(-2.,-1.75,1.08)) ;
#14771 = CARTESIAN_POINT('Origin',(-1.94142135623731,-1.60857864376269,1.07)) ;
#14772 = CARTESIAN_POINT('',(-1.94241886557342,-1.6095761530988,1.05004981327785)) ;
#14773 = CARTESIAN_POINT('',(-1.95990568186281,-1.60096027722995,1.06946130013631)) ;
#14774 = CARTESIAN_POINT('Origin',(-1.94142135623731,-1.60857864376269,1.07)) ;
#14775 = CARTESIAN_POINT('',(-1.9404238469012,-1.60758113442658,1.08995018672215)) ;
#14776 = CARTESIAN_POINT('Origin',(-1.94142135623731,-1.60857864376269,1.07)) ;
#14777 = CARTESIAN_POINT('',(-1.94916923067992,-1.59040328886133,1.06689727283974)) ;
#14778 = CARTESIAN_POINT('Origin',(-1.94142135623731,-1.60857864376269,1.07)) ;
#14779 = CARTESIAN_POINT('Origin',(-1.94142135623731,-1.60857864376269,1.07)) ;
#14780 = CARTESIAN_POINT('Origin',(-1.8,-1.55,1.06)) ;
#14781 = CARTESIAN_POINT('',(-1.80141069123172,-1.55,1.04004981327785)) ;
#14782 = CARTESIAN_POINT('',(-1.80774787444261,-1.53182464509864,1.05689727283974)) ;
#14783 = CARTESIAN_POINT('Origin',(-1.8,-1.55,1.06)) ;
#14784 = CARTESIAN_POINT('',(-1.79858930876828,-1.55,1.07995018672215)) ;
#14785 = CARTESIAN_POINT('Origin',(-1.8,-1.55,1.06)) ;
#14786 = CARTESIAN_POINT('Origin',(-1.8,-1.55,1.06)) ;
#14787 = CARTESIAN_POINT('Origin',(-1.65857864376269,-1.60857864376269,1.05)) ;
#14788 = CARTESIAN_POINT('',(-1.6595761530988,-1.60758113442658,1.03004981327785)) ;
#14789 = CARTESIAN_POINT('',(-1.65758113442658,-1.6095761530988,1.06995018672215)) ;
#14790 = CARTESIAN_POINT('Origin',(-1.65857864376269,-1.60857864376269,1.05)) ;
#14791 = CARTESIAN_POINT('Origin',(-1.65857864376269,-1.60857864376269,1.05)) ;
#14792 = CARTESIAN_POINT('Origin',(-1.6,-1.75,1.04)) ;
#14793 = CARTESIAN_POINT('',(-1.6,-1.74858930876828,1.02004981327785)) ;
#14794 = CARTESIAN_POINT('',(-1.6,-1.75141069123172,1.05995018672215)) ;
#14795 = CARTESIAN_POINT('Origin',(-1.6,-1.75,1.04)) ;
#14796 = CARTESIAN_POINT('Origin',(-1.6,-1.75,1.04)) ;
#14797 = CARTESIAN_POINT('Origin',(-1.65857864376269,-1.89142135623731,1.03)) ;
#14798 = CARTESIAN_POINT('',(-1.65758113442658,-1.8904238469012,1.01004981327785)) ;
#14799 = CARTESIAN_POINT('',(-1.6595761530988,-1.89241886557342,1.04995018672215)) ;
#14800 = CARTESIAN_POINT('Origin',(-1.65857864376269,-1.89142135623731,1.03)) ;
#14801 = CARTESIAN_POINT('Origin',(-1.65857864376269,-1.89142135623731,1.03)) ;
#14802 = CARTESIAN_POINT('Origin',(-1.8,-1.95,1.02)) ;
#14803 = CARTESIAN_POINT('',(-1.79858930876828,-1.95,1.00004981327785)) ;
#14804 = CARTESIAN_POINT('',(-1.80141069123172,-1.95,1.03995018672215)) ;
#14805 = CARTESIAN_POINT('Origin',(-1.8,-1.95,1.02)) ;
#14806 = CARTESIAN_POINT('',(-1.80774787444261,-1.96817535490136,1.02310272716026)) ;
#14807 = CARTESIAN_POINT('Origin',(-1.8,-1.95,1.02)) ;
#14808 = CARTESIAN_POINT('Origin',(-1.8,-1.95,1.02)) ;
#14809 = CARTESIAN_POINT('Origin',(-1.94142135623731,-1.89142135623731,1.01)) ;
#14810 = CARTESIAN_POINT('',(-1.9404238469012,-1.89241886557342,0.990049813277847)) ;
#14811 = CARTESIAN_POINT('',(-1.94916923067992,-1.90959671113867,1.01310272716026)) ;
#14812 = CARTESIAN_POINT('Origin',(-1.94142135623731,-1.89142135623731,1.01)) ;
#14813 = CARTESIAN_POINT('',(-1.94241886557342,-1.8904238469012,1.02995018672215)) ;
#14814 = CARTESIAN_POINT('Origin',(-1.94142135623731,-1.89142135623731,1.01)) ;
#14815 = CARTESIAN_POINT('',(-1.95990568186281,-1.89903972277005,1.01053869986369)) ;
#14816 = CARTESIAN_POINT('Origin',(-1.94142135623731,-1.89142135623731,1.01)) ;
#14817 = CARTESIAN_POINT('Origin',(-1.94142135623731,-1.89142135623731,1.01)) ;
#14818 = CARTESIAN_POINT('Origin',(-2.,-1.75,1.)) ;
#14819 = CARTESIAN_POINT('',(-2.,-1.75141069123172,0.980049813277847)) ;
#14820 = CARTESIAN_POINT('',(-2.0184843256255,-1.75761836653274,1.00053869986369)) ;
#14821 = CARTESIAN_POINT('Origin',(-2.,-1.75,1.)) ;
#14822 = CARTESIAN_POINT('',(-2.,-1.74858930876828,1.01995018672215)) ;
#14823 = CARTESIAN_POINT('Origin',(-2.,-1.75,1.)) ;
#14824 = CARTESIAN_POINT('',(-2.0184843256255,-1.74238163346726,0.999461300136314)) ;
#14825 = CARTESIAN_POINT('Origin',(-2.,-1.75,1.)) ;
#14826 = CARTESIAN_POINT('Origin',(-2.,-1.75,1.)) ;
#14827 = CARTESIAN_POINT('Origin',(-1.94142135623731,-1.60857864376269,0.99)) ;
#14828 = CARTESIAN_POINT('',(-1.94241886557342,-1.6095761530988,0.970049813277847)) ;
#14829 = CARTESIAN_POINT('',(-1.95990568186281,-1.60096027722995,0.989461300136314)) ;
#14830 = CARTESIAN_POINT('Origin',(-1.94142135623731,-1.60857864376269,0.99)) ;
#14831 = CARTESIAN_POINT('',(-1.9404238469012,-1.60758113442658,1.00995018672215)) ;
#14832 = CARTESIAN_POINT('Origin',(-1.94142135623731,-1.60857864376269,0.99)) ;
#14833 = CARTESIAN_POINT('',(-1.94916923067992,-1.59040328886133,0.986897272839741)) ;
#14834 = CARTESIAN_POINT('Origin',(-1.94142135623731,-1.60857864376269,0.99)) ;
#14835 = CARTESIAN_POINT('Origin',(-1.94142135623731,-1.60857864376269,0.99)) ;
#14836 = CARTESIAN_POINT('Origin',(-1.8,-1.55,0.98)) ;
#14837 = CARTESIAN_POINT('',(-1.80141069123172,-1.55,0.960049813277847)) ;
#14838 = CARTESIAN_POINT('',(-1.80774787444261,-1.53182464509864,0.976897272839741)) ;
#14839 = CARTESIAN_POINT('Origin',(-1.8,-1.55,0.98)) ;
#14840 = CARTESIAN_POINT('',(-1.79858930876828,-1.55,0.999950186722153)) ;
#14841 = CARTESIAN_POINT('Origin',(-1.8,-1.55,0.98)) ;
#14842 = CARTESIAN_POINT('Origin',(-1.8,-1.55,0.98)) ;
#14843 = CARTESIAN_POINT('Origin',(-1.65857864376269,-1.60857864376269,0.97)) ;
#14844 = CARTESIAN_POINT('',(-1.6595761530988,-1.60758113442658,0.950049813277848)) ;
#14845 = CARTESIAN_POINT('',(-1.65758113442658,-1.6095761530988,0.989950186722153)) ;
#14846 = CARTESIAN_POINT('Origin',(-1.65857864376269,-1.60857864376269,0.97)) ;
#14847 = CARTESIAN_POINT('Origin',(-1.65857864376269,-1.60857864376269,0.97)) ;
#14848 = CARTESIAN_POINT('Origin',(-1.6,-1.75,0.96)) ;
#14849 = CARTESIAN_POINT('',(-1.6,-1.74858930876828,0.940049813277848)) ;
#14850 = CARTESIAN_POINT('',(-1.6,-1.75141069123172,0.979950186722153)) ;
#14851 = CARTESIAN_POINT('Origin',(-1.6,-1.75,0.96)) ;
#14852 = CARTESIAN_POINT('Origin',(-1.6,-1.75,0.96)) ;
#14853 = CARTESIAN_POINT('Origin',(-1.65857864376269,-1.89142135623731,0.95)) ;
#14854 = CARTESIAN_POINT('',(-1.65758113442658,-1.8904238469012,0.930049813277848)) ;
#14855 = CARTESIAN_POINT('',(-1.6595761530988,-1.89241886557342,0.969950186722153)) ;
#14856 = CARTESIAN_POINT('Origin',(-1.65857864376269,-1.89142135623731,0.95)) ;
#14857 = CARTESIAN_POINT('Origin',(-1.65857864376269,-1.89142135623731,0.95)) ;
#14858 = CARTESIAN_POINT('Origin',(-1.8,-1.95,0.94)) ;
#14859 = CARTESIAN_POINT('',(-1.79858930876828,-1.95,0.920049813277847)) ;
#14860 = CARTESIAN_POINT('',(-1.80141069123172,-1.95,0.959950186722153)) ;
#14861 = CARTESIAN_POINT('Origin',(-1.8,-1.95,0.94)) ;
#14862 = CARTESIAN_POINT('',(-1.80774787444261,-1.96817535490136,0.943102727160259)) ;
#14863 = CARTESIAN_POINT('Origin',(-1.8,-1.95,0.94)) ;
#14864 = CARTESIAN_POINT('Origin',(-1.8,-1.95,0.94)) ;
#14865 = CARTESIAN_POINT('Origin',(-1.94142135623731,-1.89142135623731,0.93)) ;
#14866 = CARTESIAN_POINT('',(-1.9404238469012,-1.89241886557342,0.910049813277847)) ;
#14867 = CARTESIAN_POINT('',(-1.94916923067992,-1.90959671113867,0.933102727160259)) ;
#14868 = CARTESIAN_POINT('Origin',(-1.94142135623731,-1.89142135623731,0.93)) ;
#14869 = CARTESIAN_POINT('',(-1.94241886557342,-1.8904238469012,0.949950186722153)) ;
#14870 = CARTESIAN_POINT('Origin',(-1.94142135623731,-1.89142135623731,0.93)) ;
#14871 = CARTESIAN_POINT('',(-1.95990568186281,-1.89903972277005,0.930538699863687)) ;
#14872 = CARTESIAN_POINT('Origin',(-1.94142135623731,-1.89142135623731,0.93)) ;
#14873 = CARTESIAN_POINT('Origin',(-1.94142135623731,-1.89142135623731,0.93)) ;
#14874 = CARTESIAN_POINT('Origin',(-2.,-1.75,0.92)) ;
#14875 = CARTESIAN_POINT('',(-2.,-1.75141069123172,0.900049813277847)) ;
#14876 = CARTESIAN_POINT('',(-2.0184843256255,-1.75761836653274,0.920538699863687)) ;
#14877 = CARTESIAN_POINT('Origin',(-2.,-1.75,0.92)) ;
#14878 = CARTESIAN_POINT('',(-2.,-1.74858930876828,0.939950186722153)) ;
#14879 = CARTESIAN_POINT('Origin',(-2.,-1.75,0.92)) ;
#14880 = CARTESIAN_POINT('',(-2.0184843256255,-1.74238163346726,0.919461300136314)) ;
#14881 = CARTESIAN_POINT('Origin',(-2.,-1.75,0.92)) ;
#14882 = CARTESIAN_POINT('Origin',(-2.,-1.75,0.92)) ;
#14883 = CARTESIAN_POINT('Origin',(-1.94142135623731,-1.60857864376269,0.91)) ;
#14884 = CARTESIAN_POINT('',(-1.94241886557342,-1.6095761530988,0.890049813277848)) ;
#14885 = CARTESIAN_POINT('',(-1.95990568186281,-1.60096027722995,0.909461300136314)) ;
#14886 = CARTESIAN_POINT('Origin',(-1.94142135623731,-1.60857864376269,0.91)) ;
#14887 = CARTESIAN_POINT('',(-1.9404238469012,-1.60758113442658,0.929950186722153)) ;
#14888 = CARTESIAN_POINT('Origin',(-1.94142135623731,-1.60857864376269,0.91)) ;
#14889 = CARTESIAN_POINT('',(-1.94916923067992,-1.59040328886133,0.906897272839741)) ;
#14890 = CARTESIAN_POINT('Origin',(-1.94142135623731,-1.60857864376269,0.91)) ;
#14891 = CARTESIAN_POINT('Origin',(-1.94142135623731,-1.60857864376269,0.91)) ;
#14892 = CARTESIAN_POINT('Origin',(-1.8,-1.55,0.9)) ;
#14893 = CARTESIAN_POINT('',(-1.80141069123172,-1.55,0.880049813277847)) ;
#14894 = CARTESIAN_POINT('',(-1.80774787444261,-1.53182464509864,0.896897272839741)) ;
#14895 = CARTESIAN_POINT('Origin',(-1.8,-1.55,0.9)) ;
#14896 = CARTESIAN_POINT('',(-1.79858930876828,-1.55,0.919950186722153)) ;
#14897 = CARTESIAN_POINT('Origin',(-1.8,-1.55,0.9)) ;
#14898 = CARTESIAN_POINT('Origin',(-1.8,-1.55,0.9)) ;
#14899 = CARTESIAN_POINT('Origin',(-1.65857864376269,-1.60857864376269,0.89)) ;
#14900 = CARTESIAN_POINT('',(-1.6595761530988,-1.60758113442658,0.870049813277847)) ;
#14901 = CARTESIAN_POINT('',(-1.65758113442658,-1.6095761530988,0.909950186722153)) ;
#14902 = CARTESIAN_POINT('Origin',(-1.65857864376269,-1.60857864376269,0.89)) ;
#14903 = CARTESIAN_POINT('Origin',(-1.65857864376269,-1.60857864376269,0.89)) ;
#14904 = CARTESIAN_POINT('Origin',(-1.62928932188135,-1.82071067811866,1.195)) ;
#14905 = CARTESIAN_POINT('',(-1.6184843256255,-1.74238163346726,1.20053869986369)) ;
#14906 = CARTESIAN_POINT('Origin',(-1.6,-1.75,1.2)) ;
#14907 = CARTESIAN_POINT('',(-1.67391193696982,-1.87619572450464,1.1910766147446)) ;
#14908 = CARTESIAN_POINT('',(-1.64777364750685,-1.81309231158591,1.19553869986369)) ;
#14909 = CARTESIAN_POINT('',(-1.67388148147355,-1.87637536958489,1.1925685105844)) ;
#14910 = CARTESIAN_POINT('Origin',(-1.65857864376269,-1.89142135623731,1.19)) ;
#14911 = CARTESIAN_POINT('Origin',(-1.65857864376269,-1.89142135623731,1.19)) ;
#14912 = CARTESIAN_POINT('Origin',(-1.65857864376269,-1.89142135623731,1.19)) ;
#14913 = CARTESIAN_POINT('Origin',(-1.6,-1.75,1.2)) ;
#14914 = CARTESIAN_POINT('Origin',(-1.72928932188135,-1.92071067811866,1.185)) ;
#14915 = CARTESIAN_POINT('',(-1.80025685105844,-1.92872176161686,1.18363242250356)) ;
#14916 = CARTESIAN_POINT('',(-1.73703719632395,-1.90253532321729,1.18810272716026)) ;
#14917 = CARTESIAN_POINT('Origin',(-1.8,-1.95,1.18)) ;
#14918 = CARTESIAN_POINT('Origin',(-1.8,-1.95,1.18)) ;
#14919 = CARTESIAN_POINT('Origin',(-1.87071067811866,-1.92071067811865,1.175)) ;
#14920 = CARTESIAN_POINT('',(-1.87845855256126,-1.93888603302002,1.17810272716026)) ;
#14921 = CARTESIAN_POINT('Origin',(-1.94142135623731,-1.89142135623731,1.17)) ;
#14922 = CARTESIAN_POINT('Origin',(-1.97071067811865,-1.82071067811865,1.165)) ;
#14923 = CARTESIAN_POINT('',(-1.98919500374416,-1.8283290446514,1.16553869986369)) ;
#14924 = CARTESIAN_POINT('Origin',(-2.,-1.75,1.16)) ;
#14925 = CARTESIAN_POINT('Origin',(-1.97071067811865,-1.67928932188134,1.155)) ;
#14926 = CARTESIAN_POINT('',(-1.98919500374416,-1.6716709553486,1.15446130013631)) ;
#14927 = CARTESIAN_POINT('Origin',(-1.94142135623731,-1.60857864376269,1.15)) ;
#14928 = CARTESIAN_POINT('Origin',(-1.87071067811865,-1.57928932188135,1.145)) ;
#14929 = CARTESIAN_POINT('',(-1.87845855256126,-1.56111396697998,1.14189727283974)) ;
#14930 = CARTESIAN_POINT('',(-1.80025685105844,-1.57127823838314,1.13636757749644)) ;
#14931 = CARTESIAN_POINT('Origin',(-1.8,-1.55,1.14)) ;
#14932 = CARTESIAN_POINT('Origin',(-1.8,-1.55,1.14)) ;
#14933 = CARTESIAN_POINT('Origin',(-1.72928932188135,-1.57928932188135,1.135)) ;
#14934 = CARTESIAN_POINT('',(-1.67388148147355,-1.62362463041511,1.1274314894156)) ;
#14935 = CARTESIAN_POINT('',(-1.73703719632395,-1.59746467678271,1.13189727283974)) ;
#14936 = CARTESIAN_POINT('',(-1.67391193696982,-1.62380427549536,1.1289233852554)) ;
#14937 = CARTESIAN_POINT('Origin',(-1.65857864376269,-1.60857864376269,1.13)) ;
#14938 = CARTESIAN_POINT('Origin',(-1.65857864376269,-1.60857864376269,1.13)) ;
#14939 = CARTESIAN_POINT('Origin',(-1.65857864376269,-1.60857864376269,1.13)) ;
#14940 = CARTESIAN_POINT('Origin',(-1.62928932188135,-1.67928932188135,1.125)) ;
#14941 = CARTESIAN_POINT('',(-1.6216399563665,-1.75,1.12)) ;
#14942 = CARTESIAN_POINT('',(-1.64777364750685,-1.68690768841409,1.12446130013631)) ;
#14943 = CARTESIAN_POINT('Origin',(-1.6,-1.75,1.12)) ;
#14944 = CARTESIAN_POINT('Origin',(-1.6,-1.75,1.12)) ;
#14945 = CARTESIAN_POINT('Origin',(-1.62928932188135,-1.82071067811865,1.115)) ;
#14946 = CARTESIAN_POINT('',(-1.67391193696982,-1.87619572450464,1.1110766147446)) ;
#14947 = CARTESIAN_POINT('',(-1.64777364750685,-1.81309231158591,1.11553869986369)) ;
#14948 = CARTESIAN_POINT('',(-1.67388148147355,-1.87637536958489,1.1125685105844)) ;
#14949 = CARTESIAN_POINT('Origin',(-1.65857864376269,-1.89142135623731,1.11)) ;
#14950 = CARTESIAN_POINT('Origin',(-1.65857864376269,-1.89142135623731,1.11)) ;
#14951 = CARTESIAN_POINT('Origin',(-1.65857864376269,-1.89142135623731,1.11)) ;
#14952 = CARTESIAN_POINT('Origin',(-1.72928932188135,-1.92071067811865,1.105)) ;
#14953 = CARTESIAN_POINT('',(-1.80025685105844,-1.92872176161686,1.10363242250356)) ;
#14954 = CARTESIAN_POINT('',(-1.73703719632395,-1.90253532321729,1.10810272716026)) ;
#14955 = CARTESIAN_POINT('Origin',(-1.8,-1.95,1.1)) ;
#14956 = CARTESIAN_POINT('Origin',(-1.8,-1.95,1.1)) ;
#14957 = CARTESIAN_POINT('Origin',(-1.87071067811866,-1.92071067811865,1.095)) ;
#14958 = CARTESIAN_POINT('',(-1.87845855256126,-1.93888603302002,1.09810272716026)) ;
#14959 = CARTESIAN_POINT('Origin',(-1.94142135623731,-1.89142135623731,1.09)) ;
#14960 = CARTESIAN_POINT('Origin',(-1.97071067811865,-1.82071067811865,1.085)) ;
#14961 = CARTESIAN_POINT('',(-1.98919500374416,-1.8283290446514,1.08553869986369)) ;
#14962 = CARTESIAN_POINT('Origin',(-2.,-1.75,1.08)) ;
#14963 = CARTESIAN_POINT('Origin',(-1.97071067811865,-1.67928932188135,1.075)) ;
#14964 = CARTESIAN_POINT('',(-1.98919500374416,-1.6716709553486,1.07446130013631)) ;
#14965 = CARTESIAN_POINT('Origin',(-1.94142135623731,-1.60857864376269,1.07)) ;
#14966 = CARTESIAN_POINT('Origin',(-1.87071067811865,-1.57928932188135,1.065)) ;
#14967 = CARTESIAN_POINT('',(-1.87845855256126,-1.56111396697998,1.06189727283974)) ;
#14968 = CARTESIAN_POINT('',(-1.80025685105844,-1.57127823838314,1.05636757749644)) ;
#14969 = CARTESIAN_POINT('Origin',(-1.8,-1.55,1.06)) ;
#14970 = CARTESIAN_POINT('Origin',(-1.8,-1.55,1.06)) ;
#14971 = CARTESIAN_POINT('Origin',(-1.72928932188135,-1.57928932188135,1.055)) ;
#14972 = CARTESIAN_POINT('',(-1.67388148147355,-1.62362463041511,1.0474314894156)) ;
#14973 = CARTESIAN_POINT('',(-1.73703719632395,-1.59746467678271,1.05189727283974)) ;
#14974 = CARTESIAN_POINT('',(-1.67391193696982,-1.62380427549536,1.0489233852554)) ;
#14975 = CARTESIAN_POINT('Origin',(-1.65857864376269,-1.60857864376269,1.05)) ;
#14976 = CARTESIAN_POINT('Origin',(-1.65857864376269,-1.60857864376269,1.05)) ;
#14977 = CARTESIAN_POINT('Origin',(-1.65857864376269,-1.60857864376269,1.05)) ;
#14978 = CARTESIAN_POINT('Origin',(-1.62928932188135,-1.67928932188135,1.045)) ;
#14979 = CARTESIAN_POINT('',(-1.6216399563665,-1.75,1.04)) ;
#14980 = CARTESIAN_POINT('',(-1.64777364750685,-1.68690768841409,1.04446130013631)) ;
#14981 = CARTESIAN_POINT('Origin',(-1.6,-1.75,1.04)) ;
#14982 = CARTESIAN_POINT('Origin',(-1.6,-1.75,1.04)) ;
#14983 = CARTESIAN_POINT('Origin',(-1.62928932188135,-1.82071067811865,1.035)) ;
#14984 = CARTESIAN_POINT('',(-1.67391193696982,-1.87619572450464,1.0310766147446)) ;
#14985 = CARTESIAN_POINT('',(-1.64777364750685,-1.81309231158591,1.03553869986369)) ;
#14986 = CARTESIAN_POINT('',(-1.67388148147355,-1.87637536958489,1.0325685105844)) ;
#14987 = CARTESIAN_POINT('Origin',(-1.65857864376269,-1.89142135623731,1.03)) ;
#14988 = CARTESIAN_POINT('Origin',(-1.65857864376269,-1.89142135623731,1.03)) ;
#14989 = CARTESIAN_POINT('Origin',(-1.65857864376269,-1.89142135623731,1.03)) ;
#14990 = CARTESIAN_POINT('Origin',(-1.72928932188135,-1.92071067811865,1.025)) ;
#14991 = CARTESIAN_POINT('',(-1.80025685105844,-1.92872176161686,1.02363242250356)) ;
#14992 = CARTESIAN_POINT('',(-1.73703719632395,-1.90253532321729,1.02810272716026)) ;
#14993 = CARTESIAN_POINT('Origin',(-1.8,-1.95,1.02)) ;
#14994 = CARTESIAN_POINT('Origin',(-1.8,-1.95,1.02)) ;
#14995 = CARTESIAN_POINT('Origin',(-1.87071067811865,-1.92071067811865,1.015)) ;
#14996 = CARTESIAN_POINT('',(-1.87845855256126,-1.93888603302002,1.01810272716026)) ;
#14997 = CARTESIAN_POINT('Origin',(-1.94142135623731,-1.89142135623731,1.01)) ;
#14998 = CARTESIAN_POINT('Origin',(-1.97071067811865,-1.82071067811865,1.005)) ;
#14999 = CARTESIAN_POINT('',(-1.98919500374416,-1.8283290446514,1.00553869986369)) ;
#15000 = CARTESIAN_POINT('Origin',(-2.,-1.75,1.)) ;
#15001 = CARTESIAN_POINT('Origin',(-1.97071067811865,-1.67928932188135,0.995)) ;
#15002 = CARTESIAN_POINT('',(-1.98919500374416,-1.6716709553486,0.994461300136314)) ;
#15003 = CARTESIAN_POINT('Origin',(-1.94142135623731,-1.60857864376269,0.99)) ;
#15004 = CARTESIAN_POINT('Origin',(-1.87071067811865,-1.57928932188135,0.985)) ;
#15005 = CARTESIAN_POINT('',(-1.87845855256126,-1.56111396697998,0.981897272839741)) ;
#15006 = CARTESIAN_POINT('',(-1.80025685105844,-1.57127823838314,0.976367577496444)) ;
#15007 = CARTESIAN_POINT('Origin',(-1.8,-1.55,0.98)) ;
#15008 = CARTESIAN_POINT('Origin',(-1.8,-1.55,0.98)) ;
#15009 = CARTESIAN_POINT('Origin',(-1.72928932188135,-1.57928932188135,0.975)) ;
#15010 = CARTESIAN_POINT('',(-1.67388148147355,-1.62362463041511,0.967431489415601)) ;
#15011 = CARTESIAN_POINT('',(-1.73703719632395,-1.59746467678271,0.971897272839741)) ;
#15012 = CARTESIAN_POINT('',(-1.67391193696982,-1.62380427549536,0.968923385255398)) ;
#15013 = CARTESIAN_POINT('Origin',(-1.65857864376269,-1.60857864376269,0.97)) ;
#15014 = CARTESIAN_POINT('Origin',(-1.65857864376269,-1.60857864376269,0.97)) ;
#15015 = CARTESIAN_POINT('Origin',(-1.65857864376269,-1.60857864376269,0.97)) ;
#15016 = CARTESIAN_POINT('Origin',(-1.62928932188135,-1.67928932188135,0.965)) ;
#15017 = CARTESIAN_POINT('',(-1.62163995636649,-1.75,0.96)) ;
#15018 = CARTESIAN_POINT('',(-1.64777364750685,-1.68690768841409,0.964461300136314)) ;
#15019 = CARTESIAN_POINT('Origin',(-1.6,-1.75,0.96)) ;
#15020 = CARTESIAN_POINT('Origin',(-1.6,-1.75,0.96)) ;
#15021 = CARTESIAN_POINT('Origin',(-1.62928932188135,-1.82071067811865,0.955)) ;
#15022 = CARTESIAN_POINT('',(-1.67391193696982,-1.87619572450464,0.951076614744602)) ;
#15023 = CARTESIAN_POINT('',(-1.64777364750685,-1.81309231158591,0.955538699863687)) ;
#15024 = CARTESIAN_POINT('',(-1.67388148147355,-1.87637536958489,0.952568510584399)) ;
#15025 = CARTESIAN_POINT('Origin',(-1.65857864376269,-1.89142135623731,0.95)) ;
#15026 = CARTESIAN_POINT('Origin',(-1.65857864376269,-1.89142135623731,0.95)) ;
#15027 = CARTESIAN_POINT('Origin',(-1.65857864376269,-1.89142135623731,0.95)) ;
#15028 = CARTESIAN_POINT('Origin',(-1.72928932188135,-1.92071067811865,0.945)) ;
#15029 = CARTESIAN_POINT('',(-1.80025685105844,-1.92872176161686,0.943632422503557)) ;
#15030 = CARTESIAN_POINT('',(-1.73703719632395,-1.90253532321729,0.948102727160259)) ;
#15031 = CARTESIAN_POINT('Origin',(-1.8,-1.95,0.94)) ;
#15032 = CARTESIAN_POINT('Origin',(-1.8,-1.95,0.94)) ;
#15033 = CARTESIAN_POINT('Origin',(-1.87071067811865,-1.92071067811865,0.935)) ;
#15034 = CARTESIAN_POINT('',(-1.87845855256126,-1.93888603302002,0.938102727160259)) ;
#15035 = CARTESIAN_POINT('Origin',(-1.94142135623731,-1.89142135623731,0.93)) ;
#15036 = CARTESIAN_POINT('Origin',(-1.97071067811865,-1.82071067811865,0.925)) ;
#15037 = CARTESIAN_POINT('',(-1.98919500374416,-1.8283290446514,0.925538699863687)) ;
#15038 = CARTESIAN_POINT('Origin',(-2.,-1.75,0.92)) ;
#15039 = CARTESIAN_POINT('Origin',(-1.97071067811865,-1.67928932188135,0.915)) ;
#15040 = CARTESIAN_POINT('',(-1.98919500374416,-1.6716709553486,0.914461300136314)) ;
#15041 = CARTESIAN_POINT('Origin',(-1.94142135623731,-1.60857864376269,0.91)) ;
#15042 = CARTESIAN_POINT('Origin',(-1.87071067811865,-1.57928932188135,0.905)) ;
#15043 = CARTESIAN_POINT('',(-1.87845855256126,-1.56111396697998,0.901897272839741)) ;
#15044 = CARTESIAN_POINT('',(-1.80025685105844,-1.57127823838314,0.896367577496443)) ;
#15045 = CARTESIAN_POINT('Origin',(-1.8,-1.55,0.9)) ;
#15046 = CARTESIAN_POINT('Origin',(-1.8,-1.55,0.9)) ;
#15047 = CARTESIAN_POINT('Origin',(-1.72928932188135,-1.57928932188135,0.895)) ;
#15048 = CARTESIAN_POINT('',(-1.67388148147355,-1.62362463041511,0.887431489415601)) ;
#15049 = CARTESIAN_POINT('',(-1.73703719632395,-1.59746467678271,0.891897272839741)) ;
#15050 = CARTESIAN_POINT('',(-1.67391193696982,-1.62380427549536,0.888923385255398)) ;
#15051 = CARTESIAN_POINT('Origin',(-1.65857864376269,-1.60857864376269,0.89)) ;
#15052 = CARTESIAN_POINT('Origin',(-1.65857864376269,-1.60857864376269,0.89)) ;
#15053 = CARTESIAN_POINT('Origin',(-1.65857864376269,-1.60857864376269,0.89)) ;
#15054 = CARTESIAN_POINT('Origin',(-1.62928932188135,-1.67928932188135,0.885)) ;
#15055 = CARTESIAN_POINT('',(-1.6184843256255,-1.75761836653274,0.879461300136314)) ;
#15056 = CARTESIAN_POINT('',(-1.64777364750685,-1.68690768841409,0.884461300136314)) ;
#15057 = CARTESIAN_POINT('Origin',(-1.6,-1.75,0.88)) ;
#15058 = CARTESIAN_POINT('Origin',(-1.6,-1.75,0.88)) ;
#15059 = CARTESIAN_POINT('',(0.,0.,0.)) ;
#15060 = CARTESIAN_POINT('',(0.,0.,0.)) ;
#15061 = CARTESIAN_POINT('',(0.,0.,0.)) ;
#15062 = CARTESIAN_POINT('',(0.,0.,0.)) ;
#15063 = CARTESIAN_POINT('',(0.,0.,0.)) ;
#15064 = CARTESIAN_POINT('',(0.,0.,0.)) ;
#15065 = CARTESIAN_POINT('',(0.,0.,0.)) ;
#15066 = CARTESIAN_POINT('',(0.,0.,0.)) ;
#15067 = CARTESIAN_POINT('',(0.,0.,0.)) ;
#15068 = CARTESIAN_POINT('',(0.,0.,0.)) ;
#15069 = CARTESIAN_POINT('',(0.,0.,0.)) ;
#15070 = CARTESIAN_POINT('',(0.,0.,0.)) ;
#15071 = CARTESIAN_POINT('',(0.,0.,0.)) ;
#15072 = CARTESIAN_POINT('Origin',(3.65,0.,1.2)) ;
#15073 = CARTESIAN_POINT('',(3.6,-9.79717439317883E-18,1.28)) ;
#15074 = CARTESIAN_POINT('Origin',(3.6,0.,1.2)) ;
#15075 = CARTESIAN_POINT('',(3.68,9.79717439317883E-18,1.28)) ;
#15076 = CARTESIAN_POINT('',(3.65,-9.79717439317883E-18,1.28)) ;
#15077 = CARTESIAN_POINT('Origin',(3.68,0.,1.2)) ;
#15078 = CARTESIAN_POINT('Origin',(3.6,0.,1.05)) ;
#15079 = CARTESIAN_POINT('',(3.6,-0.315,0.38)) ;
#15080 = CARTESIAN_POINT('',(3.6,0.315,0.38)) ;
#15081 = CARTESIAN_POINT('',(3.6,0.,0.38)) ;
#15082 = CARTESIAN_POINT('',(3.6,-0.315,1.8)) ;
#15083 = CARTESIAN_POINT('',(3.6,-0.315,1.05)) ;
#15084 = CARTESIAN_POINT('',(3.6,0.315,1.8)) ;
#15085 = CARTESIAN_POINT('',(3.6,0.,1.8)) ;
#15086 = CARTESIAN_POINT('',(3.6,0.315,1.05)) ;
#15087 = CARTESIAN_POINT('Origin',(3.64,0.,1.8)) ;
#15088 = CARTESIAN_POINT('',(3.68,-0.315,1.8)) ;
#15089 = CARTESIAN_POINT('',(3.68,0.315,1.8)) ;
#15090 = CARTESIAN_POINT('',(3.68,0.,1.8)) ;
#15091 = CARTESIAN_POINT('',(3.64,0.315,1.8)) ;
#15092 = CARTESIAN_POINT('',(3.64,-0.315,1.8)) ;
#15093 = CARTESIAN_POINT('Origin',(3.68,0.,1.05)) ;
#15094 = CARTESIAN_POINT('',(3.68,0.315,0.38)) ;
#15095 = CARTESIAN_POINT('',(3.68,-0.315,0.38)) ;
#15096 = CARTESIAN_POINT('',(3.68,0.,0.38)) ;
#15097 = CARTESIAN_POINT('',(3.68,0.315,1.05)) ;
#15098 = CARTESIAN_POINT('',(3.68,-0.315,1.05)) ;
#15099 = CARTESIAN_POINT('Origin',(3.5,0.,0.3)) ;
#15100 = CARTESIAN_POINT('',(3.3,0.315,0.3)) ;
#15101 = CARTESIAN_POINT('',(3.7,0.315,0.3)) ;
#15102 = CARTESIAN_POINT('',(3.5,0.315,0.3)) ;
#15103 = CARTESIAN_POINT('',(3.7,-0.315,0.3)) ;
#15104 = CARTESIAN_POINT('',(3.7,0.,0.3)) ;
#15105 = CARTESIAN_POINT('',(3.3,-0.315,0.3)) ;
#15106 = CARTESIAN_POINT('',(3.5,-0.315,0.3)) ;
#15107 = CARTESIAN_POINT('',(3.3,0.,0.3)) ;
#15108 = CARTESIAN_POINT('Origin',(3.5,0.,0.38)) ;
#15109 = CARTESIAN_POINT('',(3.7,-0.315,0.38)) ;
#15110 = CARTESIAN_POINT('',(3.5,-0.315,0.38)) ;
#15111 = CARTESIAN_POINT('',(3.7,0.315,0.38)) ;
#15112 = CARTESIAN_POINT('',(3.7,0.,0.38)) ;
#15113 = CARTESIAN_POINT('',(3.5,0.315,0.38)) ;
#15114 = CARTESIAN_POINT('Origin',(3.5,0.,0.38)) ;
#15115 = CARTESIAN_POINT('',(3.3,0.315,0.38)) ;
#15116 = CARTESIAN_POINT('',(3.5,0.315,0.38)) ;
#15117 = CARTESIAN_POINT('',(3.3,-0.315,0.38)) ;
#15118 = CARTESIAN_POINT('',(3.3,0.,0.38)) ;
#15119 = CARTESIAN_POINT('',(3.5,-0.315,0.38)) ;
#15120 = CARTESIAN_POINT('Origin',(3.5,-0.315,0.34)) ;
#15121 = CARTESIAN_POINT('',(3.7,-0.315,0.34)) ;
#15122 = CARTESIAN_POINT('',(3.3,-0.315,0.34)) ;
#15123 = CARTESIAN_POINT('Origin',(3.3,0.,0.34)) ;
#15124 = CARTESIAN_POINT('',(3.3,0.315,0.34)) ;
#15125 = CARTESIAN_POINT('Origin',(3.5,0.315,0.34)) ;
#15126 = CARTESIAN_POINT('',(3.7,0.315,0.34)) ;
#15127 = CARTESIAN_POINT('Origin',(3.7,0.,0.34)) ;
#15128 = CARTESIAN_POINT('',(0.,0.,0.)) ;
#15129 = CARTESIAN_POINT('Origin',(-3.6,-0.6,0.9)) ;
#15130 = CARTESIAN_POINT('',(-3.6,-0.4,0.9)) ;
#15131 = CARTESIAN_POINT('',(-3.6,-0.8,0.9)) ;
#15132 = CARTESIAN_POINT('',(-3.6,-0.6,0.9)) ;
#15133 = CARTESIAN_POINT('',(-3.5,-0.4,0.9)) ;
#15134 = CARTESIAN_POINT('',(-3.6,-0.4,0.9)) ;
#15135 = CARTESIAN_POINT('',(-3.5,-0.8,0.9)) ;
#15136 = CARTESIAN_POINT('',(-3.5,-0.6,0.9)) ;
#15137 = CARTESIAN_POINT('',(-3.6,-0.8,0.9)) ;
#15138 = CARTESIAN_POINT('Origin',(-3.6,-0.8,0.7)) ;
#15139 = CARTESIAN_POINT('',(-3.6,-0.8,0.5)) ;
#15140 = CARTESIAN_POINT('',(-3.6,-0.8,0.675)) ;
#15141 = CARTESIAN_POINT('',(-3.5,-0.8,0.5)) ;
#15142 = CARTESIAN_POINT('',(-3.5,-0.8,0.7)) ;
#15143 = CARTESIAN_POINT('',(-3.6,-0.8,0.5)) ;
#15144 = CARTESIAN_POINT('Origin',(-3.6,-0.6,0.5)) ;
#15145 = CARTESIAN_POINT('',(-3.6,-0.4,0.5)) ;
#15146 = CARTESIAN_POINT('',(-3.6,-0.6,0.5)) ;
#15147 = CARTESIAN_POINT('',(-3.5,-0.4,0.5)) ;
#15148 = CARTESIAN_POINT('',(-3.5,-0.6,0.5)) ;
#15149 = CARTESIAN_POINT('',(-3.6,-0.4,0.5)) ;
#15150 = CARTESIAN_POINT('Origin',(-3.6,-0.4,0.7)) ;
#15151 = CARTESIAN_POINT('',(-3.6,-0.4,0.675)) ;
#15152 = CARTESIAN_POINT('',(-3.5,-0.4,0.7)) ;
#15153 = CARTESIAN_POINT('Origin',(-3.5,-0.6,0.7)) ;
#15154 = CARTESIAN_POINT('',(-3.5,-0.6,0.86)) ;
#15155 = CARTESIAN_POINT('Origin',(-3.5,-0.6,0.7)) ;
#15156 = CARTESIAN_POINT('Origin',(-3.1,-0.6,0.7)) ;
#15157 = CARTESIAN_POINT('',(-2.6,-0.6,0.86)) ;
#15158 = CARTESIAN_POINT('',(-3.1,-0.6,0.86)) ;
#15159 = CARTESIAN_POINT('Origin',(-2.6,-0.6,0.7)) ;
#15160 = CARTESIAN_POINT('Origin',(-3.1,-0.6,1.)) ;
#15161 = CARTESIAN_POINT('',(-2.6,-1.,1.)) ;
#15162 = CARTESIAN_POINT('',(-2.6,-0.2,1.)) ;
#15163 = CARTESIAN_POINT('',(-2.6,-0.6,1.)) ;
#15164 = CARTESIAN_POINT('',(-3.6,-0.2,1.)) ;
#15165 = CARTESIAN_POINT('',(-3.1,-0.2,1.)) ;
#15166 = CARTESIAN_POINT('',(-3.6,-1.,1.)) ;
#15167 = CARTESIAN_POINT('',(-3.6,-0.6,1.)) ;
#15168 = CARTESIAN_POINT('',(-3.1,-1.,1.)) ;
#15169 = CARTESIAN_POINT('Origin',(-3.1,-0.6,0.3)) ;
#15170 = CARTESIAN_POINT('',(-2.6,-0.2,0.3)) ;
#15171 = CARTESIAN_POINT('',(-2.6,-1.,0.3)) ;
#15172 = CARTESIAN_POINT('',(-2.6,-0.6,0.3)) ;
#15173 = CARTESIAN_POINT('',(-3.6,-1.,0.3)) ;
#15174 = CARTESIAN_POINT('',(-3.1,-1.,0.3)) ;
#15175 = CARTESIAN_POINT('',(-3.6,-0.2,0.3)) ;
#15176 = CARTESIAN_POINT('',(-3.6,-0.6,0.3)) ;
#15177 = CARTESIAN_POINT('',(-3.1,-0.2,0.3)) ;
#15178 = CARTESIAN_POINT('Origin',(-3.1,-1.,0.65)) ;
#15179 = CARTESIAN_POINT('',(-3.6,-1.,0.65)) ;
#15180 = CARTESIAN_POINT('',(-2.6,-1.,0.65)) ;
#15181 = CARTESIAN_POINT('Origin',(-3.6,-0.6,0.65)) ;
#15182 = CARTESIAN_POINT('',(-3.6,-0.2,0.65)) ;
#15183 = CARTESIAN_POINT('Origin',(-3.1,-0.2,0.65)) ;
#15184 = CARTESIAN_POINT('',(-2.6,-0.2,0.65)) ;
#15185 = CARTESIAN_POINT('Origin',(-2.6,-0.6,0.65)) ;
#15186 = CARTESIAN_POINT('',(0.,0.,0.)) ;
#15187 = CARTESIAN_POINT('Origin',(-3.4,-0.6,0.7)) ;
#15188 = CARTESIAN_POINT('',(-3.4,-0.6,0.85)) ;
#15189 = CARTESIAN_POINT('',(-3.4,-0.6,0.55)) ;
#15190 = CARTESIAN_POINT('Origin',(-3.4,-0.6,0.7)) ;
#15191 = CARTESIAN_POINT('Origin',(-3.4,-0.6,0.7)) ;
#15192 = CARTESIAN_POINT('Origin',(-3.4,-0.6,0.7)) ;
#15193 = CARTESIAN_POINT('Origin',(-3.4,-0.6,0.7)) ;
#15194 = CARTESIAN_POINT('Origin',(-3.15,-0.6,0.7)) ;
#15195 = CARTESIAN_POINT('',(-2.9,-0.6,0.85)) ;
#15196 = CARTESIAN_POINT('Origin',(-2.9,-0.6,0.7)) ;
#15197 = CARTESIAN_POINT('',(-3.15,-0.6,0.85)) ;
#15198 = CARTESIAN_POINT('Origin',(-2.9,-0.6,0.7)) ;
#15199 = CARTESIAN_POINT('Origin',(-2.55,-0.55,0.7)) ;
#15200 = CARTESIAN_POINT('',(-2.2,-0.55,0.725)) ;
#15201 = CARTESIAN_POINT('Origin',(-2.2,-0.55,0.7)) ;
#15202 = CARTESIAN_POINT('',(-2.9,-0.55,0.725)) ;
#15203 = CARTESIAN_POINT('',(-2.55,-0.55,0.725)) ;
#15204 = CARTESIAN_POINT('Origin',(-2.9,-0.55,0.7)) ;
#15205 = CARTESIAN_POINT('Origin',(-2.9,-0.55,0.7)) ;
#15206 = CARTESIAN_POINT('Origin',(-2.2,-0.55,0.7)) ;
#15207 = CARTESIAN_POINT('Origin',(-2.55,-0.65,0.7)) ;
#15208 = CARTESIAN_POINT('',(-2.2,-0.65,0.725)) ;
#15209 = CARTESIAN_POINT('Origin',(-2.2,-0.65,0.7)) ;
#15210 = CARTESIAN_POINT('',(-2.9,-0.65,0.725)) ;
#15211 = CARTESIAN_POINT('',(-2.55,-0.65,0.725)) ;
#15212 = CARTESIAN_POINT('Origin',(-2.9,-0.65,0.7)) ;
#15213 = CARTESIAN_POINT('Origin',(-2.9,-0.65,0.7)) ;
#15214 = CARTESIAN_POINT('Origin',(-2.2,-0.65,0.7)) ;
#15215 = CARTESIAN_POINT('',(0.,0.,0.)) ;
#15216 = CARTESIAN_POINT('Origin',(-1.7,-0.6,0.7)) ;
#15217 = CARTESIAN_POINT('',(-1.4,-0.6,0.815)) ;
#15218 = CARTESIAN_POINT('Origin',(-1.4,-0.6,0.7)) ;
#15219 = CARTESIAN_POINT('',(-2.,-0.6,0.815)) ;
#15220 = CARTESIAN_POINT('',(-1.7,-0.6,0.815)) ;
#15221 = CARTESIAN_POINT('Origin',(-2.,-0.6,0.7)) ;
#15222 = CARTESIAN_POINT('Origin',(-2.,-0.6,0.7)) ;
#15223 = CARTESIAN_POINT('Origin',(-1.4,-0.6,0.7)) ;
#15224 = CARTESIAN_POINT('Origin',(-2.1,-0.6,0.7)) ;
#15225 = CARTESIAN_POINT('',(-2.,-0.6,0.725)) ;
#15226 = CARTESIAN_POINT('Origin',(-2.,-0.6,0.7)) ;
#15227 = CARTESIAN_POINT('',(-2.2,-0.6,0.725)) ;
#15228 = CARTESIAN_POINT('',(-2.1,-0.6,0.725)) ;
#15229 = CARTESIAN_POINT('Origin',(-2.2,-0.6,0.7)) ;
#15230 = CARTESIAN_POINT('Origin',(-2.2,-0.6,0.7)) ;
#15231 = CARTESIAN_POINT('Origin',(-2.,-0.6,0.7)) ;
#15232 = CARTESIAN_POINT('Origin',(-1.2,-0.6,0.7)) ;
#15233 = CARTESIAN_POINT('',(-1.,-0.6,0.725)) ;
#15234 = CARTESIAN_POINT('Origin',(-1.,-0.6,0.7)) ;
#15235 = CARTESIAN_POINT('',(-1.4,-0.6,0.725)) ;
#15236 = CARTESIAN_POINT('',(-1.2,-0.6,0.725)) ;
#15237 = CARTESIAN_POINT('Origin',(-1.4,-0.6,0.7)) ;
#15238 = CARTESIAN_POINT('Origin',(-1.4,-0.6,0.7)) ;
#15239 = CARTESIAN_POINT('Origin',(-1.,-0.6,0.7)) ;
#15240 = CARTESIAN_POINT('',(0.,0.,0.)) ;
#15241 = CARTESIAN_POINT('Origin',(1.2,-1.8,0.85)) ;
#15242 = CARTESIAN_POINT('',(1.2,-1.61533814687381,0.7)) ;
#15243 = CARTESIAN_POINT('',(1.2,-1.8,0.81)) ;
#15244 = CARTESIAN_POINT('Origin',(1.2,-1.8,0.6)) ;
#15245 = CARTESIAN_POINT('',(1.2,-1.4,0.7)) ;
#15246 = CARTESIAN_POINT('',(1.2,-1.8,0.7)) ;
#15247 = CARTESIAN_POINT('',(1.2,-1.4,0.9)) ;
#15248 = CARTESIAN_POINT('',(1.2,-1.4,0.725)) ;
#15249 = CARTESIAN_POINT('',(1.2,-2.2,0.9)) ;
#15250 = CARTESIAN_POINT('',(1.2,-1.8,0.9)) ;
#15251 = CARTESIAN_POINT('',(1.2,-2.2,0.7)) ;
#15252 = CARTESIAN_POINT('',(1.2,-2.2,0.725)) ;
#15253 = CARTESIAN_POINT('',(1.2,-1.98466185312619,0.7)) ;
#15254 = CARTESIAN_POINT('',(1.2,-1.8,0.7)) ;
#15255 = CARTESIAN_POINT('Origin',(1.2,-1.8,0.6)) ;
#15256 = CARTESIAN_POINT('Origin',(1.6,-1.8,0.7)) ;
#15257 = CARTESIAN_POINT('',(2.,-1.98466185312619,0.7)) ;
#15258 = CARTESIAN_POINT('',(1.6,-1.98466185312619,0.7)) ;
#15259 = CARTESIAN_POINT('',(2.,-2.2,0.7)) ;
#15260 = CARTESIAN_POINT('',(1.6,-2.2,0.7)) ;
#15261 = CARTESIAN_POINT('',(2.,-1.8,0.7)) ;
#15262 = CARTESIAN_POINT('Origin',(1.6,-1.8,0.7)) ;
#15263 = CARTESIAN_POINT('',(2.,-1.61533814687381,0.7)) ;
#15264 = CARTESIAN_POINT('',(1.6,-1.61533814687381,0.7)) ;
#15265 = CARTESIAN_POINT('',(2.,-1.4,0.7)) ;
#15266 = CARTESIAN_POINT('',(2.,-1.8,0.7)) ;
#15267 = CARTESIAN_POINT('',(1.6,-1.4,0.7)) ;
#15268 = CARTESIAN_POINT('Origin',(2.,-1.8,0.85)) ;
#15269 = CARTESIAN_POINT('',(2.,-1.8,0.81)) ;
#15270 = CARTESIAN_POINT('Origin',(2.,-1.8,0.6)) ;
#15271 = CARTESIAN_POINT('',(2.,-2.2,0.9)) ;
#15272 = CARTESIAN_POINT('',(2.,-2.2,0.725)) ;
#15273 = CARTESIAN_POINT('',(2.,-1.4,0.9)) ;
#15274 = CARTESIAN_POINT('',(2.,-1.8,0.9)) ;
#15275 = CARTESIAN_POINT('',(2.,-1.4,0.725)) ;
#15276 = CARTESIAN_POINT('Origin',(2.,-1.8,0.6)) ;
#15277 = CARTESIAN_POINT('Origin',(1.6,-1.4,0.6)) ;
#15278 = CARTESIAN_POINT('',(2.2,-1.4,0.9)) ;
#15279 = CARTESIAN_POINT('',(1.6,-1.4,0.9)) ;
#15280 = CARTESIAN_POINT('',(2.2,-1.4,0.3)) ;
#15281 = CARTESIAN_POINT('',(2.2,-1.4,0.6)) ;
#15282 = CARTESIAN_POINT('',(1.,-1.4,0.3)) ;
#15283 = CARTESIAN_POINT('',(1.6,-1.4,0.3)) ;
#15284 = CARTESIAN_POINT('',(1.,-1.4,0.9)) ;
#15285 = CARTESIAN_POINT('',(1.,-1.4,0.6)) ;
#15286 = CARTESIAN_POINT('',(1.6,-1.4,0.9)) ;
#15287 = CARTESIAN_POINT('Origin',(1.6,-1.8,0.9)) ;
#15288 = CARTESIAN_POINT('',(2.2,-2.2,0.9)) ;
#15289 = CARTESIAN_POINT('',(1.6,-2.2,0.9)) ;
#15290 = CARTESIAN_POINT('',(2.2,-1.8,0.9)) ;
#15291 = CARTESIAN_POINT('Origin',(1.6,-1.8,0.9)) ;
#15292 = CARTESIAN_POINT('',(1.,-2.2,0.9)) ;
#15293 = CARTESIAN_POINT('',(1.,-1.8,0.9)) ;
#15294 = CARTESIAN_POINT('',(1.6,-2.2,0.9)) ;
#15295 = CARTESIAN_POINT('Origin',(1.6,-1.8,0.6)) ;
#15296 = CARTESIAN_POINT('',(1.,-1.8,0.81)) ;
#15297 = CARTESIAN_POINT('Origin',(1.,-1.8,0.6)) ;
#15298 = CARTESIAN_POINT('',(1.6,-1.8,0.81)) ;
#15299 = CARTESIAN_POINT('',(2.2,-1.8,0.81)) ;
#15300 = CARTESIAN_POINT('',(1.6,-1.8,0.81)) ;
#15301 = CARTESIAN_POINT('Origin',(2.2,-1.8,0.6)) ;
#15302 = CARTESIAN_POINT('Origin',(1.6,-1.8,0.3)) ;
#15303 = CARTESIAN_POINT('',(2.2,-2.2,0.3)) ;
#15304 = CARTESIAN_POINT('',(2.2,-1.8,0.3)) ;
#15305 = CARTESIAN_POINT('',(1.,-2.2,0.3)) ;
#15306 = CARTESIAN_POINT('',(1.6,-2.2,0.3)) ;
#15307 = CARTESIAN_POINT('',(1.,-1.8,0.3)) ;
#15308 = CARTESIAN_POINT('Origin',(1.6,-2.2,0.6)) ;
#15309 = CARTESIAN_POINT('',(1.,-2.2,0.6)) ;
#15310 = CARTESIAN_POINT('',(2.2,-2.2,0.6)) ;
#15311 = CARTESIAN_POINT('Origin',(1.,-1.8,0.6)) ;
#15312 = CARTESIAN_POINT('Origin',(2.2,-1.8,0.6)) ;
#15313 = CARTESIAN_POINT('',(0.,0.,0.)) ;
#15314 = CARTESIAN_POINT('Origin',(1.6,-1.8,0.6)) ;
#15315 = CARTESIAN_POINT('',(2.1,-1.8,0.8)) ;
#15316 = CARTESIAN_POINT('Origin',(2.1,-1.8,0.6)) ;
#15317 = CARTESIAN_POINT('',(1.1,-1.8,0.8)) ;
#15318 = CARTESIAN_POINT('',(1.6,-1.8,0.8)) ;
#15319 = CARTESIAN_POINT('Origin',(1.1,-1.8,0.6)) ;
#15320 = CARTESIAN_POINT('Origin',(1.1,-1.8,0.6)) ;
#15321 = CARTESIAN_POINT('Origin',(2.1,-1.8,0.6)) ;
#15322 = CARTESIAN_POINT('Origin',(0.8,-1.8,0.6)) ;
#15323 = CARTESIAN_POINT('',(1.1,-1.8,0.64)) ;
#15324 = CARTESIAN_POINT('Origin',(1.1,-1.8,0.6)) ;
#15325 = CARTESIAN_POINT('',(0.5,-1.8,0.64)) ;
#15326 = CARTESIAN_POINT('',(0.8,-1.8,0.64)) ;
#15327 = CARTESIAN_POINT('Origin',(0.5,-1.8,0.6)) ;
#15328 = CARTESIAN_POINT('Origin',(0.5,-1.8,0.6)) ;
#15329 = CARTESIAN_POINT('Origin',(1.1,-1.8,0.6)) ;
#15330 = CARTESIAN_POINT('Origin',(2.4,-1.8,0.6)) ;
#15331 = CARTESIAN_POINT('',(2.7,-1.8,0.64)) ;
#15332 = CARTESIAN_POINT('Origin',(2.7,-1.8,0.6)) ;
#15333 = CARTESIAN_POINT('',(2.1,-1.8,0.64)) ;
#15334 = CARTESIAN_POINT('',(2.4,-1.8,0.64)) ;
#15335 = CARTESIAN_POINT('Origin',(2.1,-1.8,0.6)) ;
#15336 = CARTESIAN_POINT('Origin',(2.1,-1.8,0.6)) ;
#15337 = CARTESIAN_POINT('Origin',(2.7,-1.8,0.6)) ;
#15338 = CARTESIAN_POINT('',(0.,0.,0.)) ;
#15339 = CARTESIAN_POINT('Origin',(2.5,-1.6,-0.4)) ;
#15340 = CARTESIAN_POINT('',(4.,-1.6,-0.11)) ;
#15341 = CARTESIAN_POINT('Origin',(4.,-1.6,-0.4)) ;
#15342 = CARTESIAN_POINT('',(1.,-1.6,-0.11)) ;
#15343 = CARTESIAN_POINT('',(2.5,-1.6,-0.11)) ;
#15344 = CARTESIAN_POINT('Origin',(1.,-1.6,-0.4)) ;
#15345 = CARTESIAN_POINT('Origin',(1.,-1.6,-0.4)) ;
#15346 = CARTESIAN_POINT('Origin',(4.,-1.6,-0.4)) ;
#15347 = CARTESIAN_POINT('',(0.,0.,0.)) ;
#15348 = CARTESIAN_POINT('',(0.,-1.4,0.)) ;
#15349 = CARTESIAN_POINT('',(0.,1.4,0.)) ;
#15350 = CARTESIAN_POINT('',(0.,0.,0.)) ;
#15351 = CARTESIAN_POINT('',(0.,0.,0.)) ;
#15352 = CARTESIAN_POINT('',(0.,0.,0.)) ;
#15353 = CARTESIAN_POINT('',(0.,0.,0.)) ;
#15354 = CARTESIAN_POINT('',(0.,0.,0.)) ;
#15355 = CARTESIAN_POINT('',(0.,0.,0.)) ;
#15356 = CARTESIAN_POINT('',(0.,0.,0.)) ;
#15357 = CARTESIAN_POINT('',(0.,0.,0.)) ;
#15358 = CARTESIAN_POINT('Origin',(0.,0.,0.4)) ;
#15359 = CARTESIAN_POINT('',(-0.15,-1.83697019872103E-17,0.8)) ;
#15360 = CARTESIAN_POINT('Origin',(0.,0.,0.8)) ;
#15361 = CARTESIAN_POINT('',(-0.15,-1.83697019872103E-17,0.)) ;
#15362 = CARTESIAN_POINT('',(-0.15,-1.83697019872103E-17,0.4)) ;
#15363 = CARTESIAN_POINT('Origin',(0.,0.,0.)) ;
#15364 = CARTESIAN_POINT('Origin',(0.,0.,0.8)) ;
#15365 = CARTESIAN_POINT('Origin',(0.,0.,-0.1)) ;
#15366 = CARTESIAN_POINT('',(-0.275,-3.36777869765522E-17,0.)) ;
#15367 = CARTESIAN_POINT('Origin',(0.,0.,0.)) ;
#15368 = CARTESIAN_POINT('',(-0.275,-3.36777869765522E-17,-0.2)) ;
#15369 = CARTESIAN_POINT('',(-0.275,-3.36777869765522E-17,-0.1)) ;
#15370 = CARTESIAN_POINT('Origin',(0.,0.,-0.2)) ;
#15371 = CARTESIAN_POINT('Origin',(0.,0.,-0.2)) ;
#15372 = CARTESIAN_POINT('Origin',(0.,0.,0.)) ;
#15373 = CARTESIAN_POINT('',(0.,0.,0.)) ;
#15374 = CARTESIAN_POINT('Origin',(0.,0.,0.4)) ;
#15375 = CARTESIAN_POINT('',(-0.15,-1.83697019872103E-17,0.8)) ;
#15376 = CARTESIAN_POINT('Origin',(0.,0.,0.8)) ;
#15377 = CARTESIAN_POINT('',(-0.15,-1.83697019872103E-17,0.)) ;
#15378 = CARTESIAN_POINT('',(-0.15,-1.83697019872103E-17,0.4)) ;
#15379 = CARTESIAN_POINT('Origin',(0.,0.,0.)) ;
#15380 = CARTESIAN_POINT('Origin',(0.,0.,0.8)) ;
#15381 = CARTESIAN_POINT('Origin',(0.,0.,-0.1)) ;
#15382 = CARTESIAN_POINT('',(-0.275,-3.36777869765522E-17,0.)) ;
#15383 = CARTESIAN_POINT('Origin',(0.,0.,0.)) ;
#15384 = CARTESIAN_POINT('',(-0.275,-3.36777869765522E-17,-0.2)) ;
#15385 = CARTESIAN_POINT('',(-0.275,-3.36777869765522E-17,-0.1)) ;
#15386 = CARTESIAN_POINT('Origin',(0.,0.,-0.2)) ;
#15387 = CARTESIAN_POINT('Origin',(0.,0.,-0.2)) ;
#15388 = CARTESIAN_POINT('Origin',(0.,0.,0.)) ;
#15389 = CARTESIAN_POINT('',(2.8,-1.05,-0.6)) ;
#15390 = CARTESIAN_POINT('',(3.6,-1.05,-0.6)) ;
#15391 = CARTESIAN_POINT('',(0.,2.85,0.)) ;
#15392 = CARTESIAN_POINT('',(0.,-2.85,0.)) ;
#15393 = CARTESIAN_POINT('',(0.,0.,0.)) ;
#15394 = CARTESIAN_POINT('',(0.,0.,0.)) ;
#15395 = CARTESIAN_POINT('',(0.,0.,0.)) ;
#15396 = CARTESIAN_POINT('',(0.,0.,0.)) ;
#15397 = CARTESIAN_POINT('',(0.,0.,0.)) ;
#15398 = CARTESIAN_POINT('',(0.,0.,0.)) ;
#15399 = UNCERTAINTY_MEASURE_WITH_UNIT(LENGTH_MEASURE(0.001),#15485,
'DISTANCE_ACCURACY_VALUE',
'Maximum model space distance between geometric entities at asserted c
onnectivities') ;
#15400 = UNCERTAINTY_MEASURE_WITH_UNIT(LENGTH_MEASURE(0.001),#15485,
'DISTANCE_ACCURACY_VALUE',
'Maximum model space distance between geometric entities at asserted c
onnectivities') ;
#15401 = UNCERTAINTY_MEASURE_WITH_UNIT(LENGTH_MEASURE(0.001),#15485,
'DISTANCE_ACCURACY_VALUE',
'Maximum model space distance between geometric entities at asserted c
onnectivities') ;
#15402 = UNCERTAINTY_MEASURE_WITH_UNIT(LENGTH_MEASURE(0.001),#15485,
'DISTANCE_ACCURACY_VALUE',
'Maximum model space distance between geometric entities at asserted c
onnectivities') ;
#15403 = UNCERTAINTY_MEASURE_WITH_UNIT(LENGTH_MEASURE(0.001),#15485,
'DISTANCE_ACCURACY_VALUE',
'Maximum model space distance between geometric entities at asserted c
onnectivities') ;
#15404 = UNCERTAINTY_MEASURE_WITH_UNIT(LENGTH_MEASURE(0.001),#15485,
'DISTANCE_ACCURACY_VALUE',
'Maximum model space distance between geometric entities at asserted c
onnectivities') ;
#15405 = UNCERTAINTY_MEASURE_WITH_UNIT(LENGTH_MEASURE(0.001),#15485,
'DISTANCE_ACCURACY_VALUE',
'Maximum model space distance between geometric entities at asserted c
onnectivities') ;
#15406 = UNCERTAINTY_MEASURE_WITH_UNIT(LENGTH_MEASURE(0.001),#15485,
'DISTANCE_ACCURACY_VALUE',
'Maximum model space distance between geometric entities at asserted c
onnectivities') ;
#15407 = UNCERTAINTY_MEASURE_WITH_UNIT(LENGTH_MEASURE(0.001),#15485,
'DISTANCE_ACCURACY_VALUE',
'Maximum model space distance between geometric entities at asserted c
onnectivities') ;
#15408 = UNCERTAINTY_MEASURE_WITH_UNIT(LENGTH_MEASURE(0.001),#15485,
'DISTANCE_ACCURACY_VALUE',
'Maximum model space distance between geometric entities at asserted c
onnectivities') ;
#15409 = UNCERTAINTY_MEASURE_WITH_UNIT(LENGTH_MEASURE(0.001),#15485,
'DISTANCE_ACCURACY_VALUE',
'Maximum model space distance between geometric entities at asserted c
onnectivities') ;
#15410 = UNCERTAINTY_MEASURE_WITH_UNIT(LENGTH_MEASURE(0.001),#15485,
'DISTANCE_ACCURACY_VALUE',
'Maximum model space distance between geometric entities at asserted c
onnectivities') ;
#15411 = UNCERTAINTY_MEASURE_WITH_UNIT(LENGTH_MEASURE(0.001),#15485,
'DISTANCE_ACCURACY_VALUE',
'Maximum model space distance between geometric entities at asserted c
onnectivities') ;
#15412 = UNCERTAINTY_MEASURE_WITH_UNIT(LENGTH_MEASURE(0.001),#15485,
'DISTANCE_ACCURACY_VALUE',
'Maximum model space distance between geometric entities at asserted c
onnectivities') ;
#15413 = UNCERTAINTY_MEASURE_WITH_UNIT(LENGTH_MEASURE(0.001),#15485,
'DISTANCE_ACCURACY_VALUE',
'Maximum model space distance between geometric entities at asserted c
onnectivities') ;
#15414 = UNCERTAINTY_MEASURE_WITH_UNIT(LENGTH_MEASURE(0.001),#15485,
'DISTANCE_ACCURACY_VALUE',
'Maximum model space distance between geometric entities at asserted c
onnectivities') ;
#15415 = UNCERTAINTY_MEASURE_WITH_UNIT(LENGTH_MEASURE(0.001),#15485,
'DISTANCE_ACCURACY_VALUE',
'Maximum model space distance between geometric entities at asserted c
onnectivities') ;
#15416 = UNCERTAINTY_MEASURE_WITH_UNIT(LENGTH_MEASURE(0.001),#15485,
'DISTANCE_ACCURACY_VALUE',
'Maximum model space distance between geometric entities at asserted c
onnectivities') ;
#15417 = UNCERTAINTY_MEASURE_WITH_UNIT(LENGTH_MEASURE(0.001),#15485,
'DISTANCE_ACCURACY_VALUE',
'Maximum model space distance between geometric entities at asserted c
onnectivities') ;
#15418 = UNCERTAINTY_MEASURE_WITH_UNIT(LENGTH_MEASURE(0.001),#15485,
'DISTANCE_ACCURACY_VALUE',
'Maximum model space distance between geometric entities at asserted c
onnectivities') ;
#15419 = UNCERTAINTY_MEASURE_WITH_UNIT(LENGTH_MEASURE(0.001),#15485,
'DISTANCE_ACCURACY_VALUE',
'Maximum model space distance between geometric entities at asserted c
onnectivities') ;
#15420 = UNCERTAINTY_MEASURE_WITH_UNIT(LENGTH_MEASURE(0.001),#15485,
'DISTANCE_ACCURACY_VALUE',
'Maximum model space distance between geometric entities at asserted c
onnectivities') ;
#15421 = UNCERTAINTY_MEASURE_WITH_UNIT(LENGTH_MEASURE(0.001),#15485,
'DISTANCE_ACCURACY_VALUE',
'Maximum model space distance between geometric entities at asserted c
onnectivities') ;
#15422 = UNCERTAINTY_MEASURE_WITH_UNIT(LENGTH_MEASURE(0.001),#15485,
'DISTANCE_ACCURACY_VALUE',
'Maximum model space distance between geometric entities at asserted c
onnectivities') ;
#15423 = UNCERTAINTY_MEASURE_WITH_UNIT(LENGTH_MEASURE(0.001),#15485,
'DISTANCE_ACCURACY_VALUE',
'Maximum model space distance between geometric entities at asserted c
onnectivities') ;
#15424 = UNCERTAINTY_MEASURE_WITH_UNIT(LENGTH_MEASURE(0.001),#15485,
'DISTANCE_ACCURACY_VALUE',
'Maximum model space distance between geometric entities at asserted c
onnectivities') ;
#15425 = UNCERTAINTY_MEASURE_WITH_UNIT(LENGTH_MEASURE(0.001),#15485,
'DISTANCE_ACCURACY_VALUE',
'Maximum model space distance between geometric entities at asserted c
onnectivities') ;
#15426 = UNCERTAINTY_MEASURE_WITH_UNIT(LENGTH_MEASURE(0.001),#15485,
'DISTANCE_ACCURACY_VALUE',
'Maximum model space distance between geometric entities at asserted c
onnectivities') ;
#15427 = UNCERTAINTY_MEASURE_WITH_UNIT(LENGTH_MEASURE(0.001),#15485,
'DISTANCE_ACCURACY_VALUE',
'Maximum model space distance between geometric entities at asserted c
onnectivities') ;
#15428 = UNCERTAINTY_MEASURE_WITH_UNIT(LENGTH_MEASURE(0.001),#15485,
'DISTANCE_ACCURACY_VALUE',
'Maximum model space distance between geometric entities at asserted c
onnectivities') ;
#15429 = UNCERTAINTY_MEASURE_WITH_UNIT(LENGTH_MEASURE(0.001),#15485,
'DISTANCE_ACCURACY_VALUE',
'Maximum model space distance between geometric entities at asserted c
onnectivities') ;
#15430 = UNCERTAINTY_MEASURE_WITH_UNIT(LENGTH_MEASURE(0.001),#15485,
'DISTANCE_ACCURACY_VALUE',
'Maximum model space distance between geometric entities at asserted c
onnectivities') ;
#15431 = UNCERTAINTY_MEASURE_WITH_UNIT(LENGTH_MEASURE(0.001),#15485,
'DISTANCE_ACCURACY_VALUE',
'Maximum model space distance between geometric entities at asserted c
onnectivities') ;
#15432 = UNCERTAINTY_MEASURE_WITH_UNIT(LENGTH_MEASURE(0.001),#15485,
'DISTANCE_ACCURACY_VALUE',
'Maximum model space distance between geometric entities at asserted c
onnectivities') ;
#15433 = UNCERTAINTY_MEASURE_WITH_UNIT(LENGTH_MEASURE(0.001),#15485,
'DISTANCE_ACCURACY_VALUE',
'Maximum model space distance between geometric entities at asserted c
onnectivities') ;
#15434 = UNCERTAINTY_MEASURE_WITH_UNIT(LENGTH_MEASURE(0.001),#15485,
'DISTANCE_ACCURACY_VALUE',
'Maximum model space distance between geometric entities at asserted c
onnectivities') ;
#15435 = UNCERTAINTY_MEASURE_WITH_UNIT(LENGTH_MEASURE(0.001),#15485,
'DISTANCE_ACCURACY_VALUE',
'Maximum model space distance between geometric entities at asserted c
onnectivities') ;
#15436 = UNCERTAINTY_MEASURE_WITH_UNIT(LENGTH_MEASURE(0.001),#15485,
'DISTANCE_ACCURACY_VALUE',
'Maximum model space distance between geometric entities at asserted c
onnectivities') ;
#15437 = UNCERTAINTY_MEASURE_WITH_UNIT(LENGTH_MEASURE(0.001),#15485,
'DISTANCE_ACCURACY_VALUE',
'Maximum model space distance between geometric entities at asserted c
onnectivities') ;
#15438 = UNCERTAINTY_MEASURE_WITH_UNIT(LENGTH_MEASURE(0.001),#15485,
'DISTANCE_ACCURACY_VALUE',
'Maximum model space distance between geometric entities at asserted c
onnectivities') ;
#15439 = UNCERTAINTY_MEASURE_WITH_UNIT(LENGTH_MEASURE(0.001),#15485,
'DISTANCE_ACCURACY_VALUE',
'Maximum model space distance between geometric entities at asserted c
onnectivities') ;
#15440 = UNCERTAINTY_MEASURE_WITH_UNIT(LENGTH_MEASURE(0.001),#15485,
'DISTANCE_ACCURACY_VALUE',
'Maximum model space distance between geometric entities at asserted c
onnectivities') ;
#15441 = UNCERTAINTY_MEASURE_WITH_UNIT(LENGTH_MEASURE(0.001),#15485,
'DISTANCE_ACCURACY_VALUE',
'Maximum model space distance between geometric entities at asserted c
onnectivities') ;
#15442 = (
GEOMETRIC_REPRESENTATION_CONTEXT(3)
GLOBAL_UNCERTAINTY_ASSIGNED_CONTEXT((#15399))
GLOBAL_UNIT_ASSIGNED_CONTEXT((#15485,#15487,#15488))
REPRESENTATION_CONTEXT('','3D')
) ;
#15443 = (
GEOMETRIC_REPRESENTATION_CONTEXT(3)
GLOBAL_UNCERTAINTY_ASSIGNED_CONTEXT((#15400))
GLOBAL_UNIT_ASSIGNED_CONTEXT((#15485,#15487,#15488))
REPRESENTATION_CONTEXT('','3D')
) ;
#15444 = (
GEOMETRIC_REPRESENTATION_CONTEXT(3)
GLOBAL_UNCERTAINTY_ASSIGNED_CONTEXT((#15401))
GLOBAL_UNIT_ASSIGNED_CONTEXT((#15485,#15487,#15488))
REPRESENTATION_CONTEXT('','3D')
) ;
#15445 = (
GEOMETRIC_REPRESENTATION_CONTEXT(3)
GLOBAL_UNCERTAINTY_ASSIGNED_CONTEXT((#15402))
GLOBAL_UNIT_ASSIGNED_CONTEXT((#15485,#15487,#15488))
REPRESENTATION_CONTEXT('','3D')
) ;
#15446 = (
GEOMETRIC_REPRESENTATION_CONTEXT(3)
GLOBAL_UNCERTAINTY_ASSIGNED_CONTEXT((#15403))
GLOBAL_UNIT_ASSIGNED_CONTEXT((#15485,#15487,#15488))
REPRESENTATION_CONTEXT('','3D')
) ;
#15447 = (
GEOMETRIC_REPRESENTATION_CONTEXT(3)
GLOBAL_UNCERTAINTY_ASSIGNED_CONTEXT((#15404))
GLOBAL_UNIT_ASSIGNED_CONTEXT((#15485,#15487,#15488))
REPRESENTATION_CONTEXT('','3D')
) ;
#15448 = (
GEOMETRIC_REPRESENTATION_CONTEXT(3)
GLOBAL_UNCERTAINTY_ASSIGNED_CONTEXT((#15405))
GLOBAL_UNIT_ASSIGNED_CONTEXT((#15485,#15487,#15488))
REPRESENTATION_CONTEXT('','3D')
) ;
#15449 = (
GEOMETRIC_REPRESENTATION_CONTEXT(3)
GLOBAL_UNCERTAINTY_ASSIGNED_CONTEXT((#15406))
GLOBAL_UNIT_ASSIGNED_CONTEXT((#15485,#15487,#15488))
REPRESENTATION_CONTEXT('','3D')
) ;
#15450 = (
GEOMETRIC_REPRESENTATION_CONTEXT(3)
GLOBAL_UNCERTAINTY_ASSIGNED_CONTEXT((#15407))
GLOBAL_UNIT_ASSIGNED_CONTEXT((#15485,#15487,#15488))
REPRESENTATION_CONTEXT('','3D')
) ;
#15451 = (
GEOMETRIC_REPRESENTATION_CONTEXT(3)
GLOBAL_UNCERTAINTY_ASSIGNED_CONTEXT((#15408))
GLOBAL_UNIT_ASSIGNED_CONTEXT((#15485,#15487,#15488))
REPRESENTATION_CONTEXT('','3D')
) ;
#15452 = (
GEOMETRIC_REPRESENTATION_CONTEXT(3)
GLOBAL_UNCERTAINTY_ASSIGNED_CONTEXT((#15409))
GLOBAL_UNIT_ASSIGNED_CONTEXT((#15485,#15487,#15488))
REPRESENTATION_CONTEXT('','3D')
) ;
#15453 = (
GEOMETRIC_REPRESENTATION_CONTEXT(3)
GLOBAL_UNCERTAINTY_ASSIGNED_CONTEXT((#15410))
GLOBAL_UNIT_ASSIGNED_CONTEXT((#15485,#15487,#15488))
REPRESENTATION_CONTEXT('','3D')
) ;
#15454 = (
GEOMETRIC_REPRESENTATION_CONTEXT(3)
GLOBAL_UNCERTAINTY_ASSIGNED_CONTEXT((#15411))
GLOBAL_UNIT_ASSIGNED_CONTEXT((#15485,#15487,#15488))
REPRESENTATION_CONTEXT('','3D')
) ;
#15455 = (
GEOMETRIC_REPRESENTATION_CONTEXT(3)
GLOBAL_UNCERTAINTY_ASSIGNED_CONTEXT((#15412))
GLOBAL_UNIT_ASSIGNED_CONTEXT((#15485,#15487,#15488))
REPRESENTATION_CONTEXT('','3D')
) ;
#15456 = (
GEOMETRIC_REPRESENTATION_CONTEXT(3)
GLOBAL_UNCERTAINTY_ASSIGNED_CONTEXT((#15413))
GLOBAL_UNIT_ASSIGNED_CONTEXT((#15485,#15487,#15488))
REPRESENTATION_CONTEXT('','3D')
) ;
#15457 = (
GEOMETRIC_REPRESENTATION_CONTEXT(3)
GLOBAL_UNCERTAINTY_ASSIGNED_CONTEXT((#15414))
GLOBAL_UNIT_ASSIGNED_CONTEXT((#15485,#15487,#15488))
REPRESENTATION_CONTEXT('','3D')
) ;
#15458 = (
GEOMETRIC_REPRESENTATION_CONTEXT(3)
GLOBAL_UNCERTAINTY_ASSIGNED_CONTEXT((#15415))
GLOBAL_UNIT_ASSIGNED_CONTEXT((#15485,#15487,#15488))
REPRESENTATION_CONTEXT('','3D')
) ;
#15459 = (
GEOMETRIC_REPRESENTATION_CONTEXT(3)
GLOBAL_UNCERTAINTY_ASSIGNED_CONTEXT((#15416))
GLOBAL_UNIT_ASSIGNED_CONTEXT((#15485,#15487,#15488))
REPRESENTATION_CONTEXT('','3D')
) ;
#15460 = (
GEOMETRIC_REPRESENTATION_CONTEXT(3)
GLOBAL_UNCERTAINTY_ASSIGNED_CONTEXT((#15417))
GLOBAL_UNIT_ASSIGNED_CONTEXT((#15485,#15487,#15488))
REPRESENTATION_CONTEXT('','3D')
) ;
#15461 = (
GEOMETRIC_REPRESENTATION_CONTEXT(3)
GLOBAL_UNCERTAINTY_ASSIGNED_CONTEXT((#15418))
GLOBAL_UNIT_ASSIGNED_CONTEXT((#15485,#15487,#15488))
REPRESENTATION_CONTEXT('','3D')
) ;
#15462 = (
GEOMETRIC_REPRESENTATION_CONTEXT(3)
GLOBAL_UNCERTAINTY_ASSIGNED_CONTEXT((#15419))
GLOBAL_UNIT_ASSIGNED_CONTEXT((#15485,#15487,#15488))
REPRESENTATION_CONTEXT('','3D')
) ;
#15463 = (
GEOMETRIC_REPRESENTATION_CONTEXT(3)
GLOBAL_UNCERTAINTY_ASSIGNED_CONTEXT((#15420))
GLOBAL_UNIT_ASSIGNED_CONTEXT((#15485,#15487,#15488))
REPRESENTATION_CONTEXT('','3D')
) ;
#15464 = (
GEOMETRIC_REPRESENTATION_CONTEXT(3)
GLOBAL_UNCERTAINTY_ASSIGNED_CONTEXT((#15421))
GLOBAL_UNIT_ASSIGNED_CONTEXT((#15485,#15487,#15488))
REPRESENTATION_CONTEXT('','3D')
) ;
#15465 = (
GEOMETRIC_REPRESENTATION_CONTEXT(3)
GLOBAL_UNCERTAINTY_ASSIGNED_CONTEXT((#15422))
GLOBAL_UNIT_ASSIGNED_CONTEXT((#15485,#15487,#15488))
REPRESENTATION_CONTEXT('','3D')
) ;
#15466 = (
GEOMETRIC_REPRESENTATION_CONTEXT(3)
GLOBAL_UNCERTAINTY_ASSIGNED_CONTEXT((#15423))
GLOBAL_UNIT_ASSIGNED_CONTEXT((#15485,#15487,#15488))
REPRESENTATION_CONTEXT('','3D')
) ;
#15467 = (
GEOMETRIC_REPRESENTATION_CONTEXT(3)
GLOBAL_UNCERTAINTY_ASSIGNED_CONTEXT((#15424))
GLOBAL_UNIT_ASSIGNED_CONTEXT((#15485,#15487,#15488))
REPRESENTATION_CONTEXT('','3D')
) ;
#15468 = (
GEOMETRIC_REPRESENTATION_CONTEXT(3)
GLOBAL_UNCERTAINTY_ASSIGNED_CONTEXT((#15425))
GLOBAL_UNIT_ASSIGNED_CONTEXT((#15485,#15487,#15488))
REPRESENTATION_CONTEXT('','3D')
) ;
#15469 = (
GEOMETRIC_REPRESENTATION_CONTEXT(3)
GLOBAL_UNCERTAINTY_ASSIGNED_CONTEXT((#15426))
GLOBAL_UNIT_ASSIGNED_CONTEXT((#15485,#15487,#15488))
REPRESENTATION_CONTEXT('','3D')
) ;
#15470 = (
GEOMETRIC_REPRESENTATION_CONTEXT(3)
GLOBAL_UNCERTAINTY_ASSIGNED_CONTEXT((#15427))
GLOBAL_UNIT_ASSIGNED_CONTEXT((#15485,#15487,#15488))
REPRESENTATION_CONTEXT('','3D')
) ;
#15471 = (
GEOMETRIC_REPRESENTATION_CONTEXT(3)
GLOBAL_UNCERTAINTY_ASSIGNED_CONTEXT((#15428))
GLOBAL_UNIT_ASSIGNED_CONTEXT((#15485,#15487,#15488))
REPRESENTATION_CONTEXT('','3D')
) ;
#15472 = (
GEOMETRIC_REPRESENTATION_CONTEXT(3)
GLOBAL_UNCERTAINTY_ASSIGNED_CONTEXT((#15429))
GLOBAL_UNIT_ASSIGNED_CONTEXT((#15485,#15487,#15488))
REPRESENTATION_CONTEXT('','3D')
) ;
#15473 = (
GEOMETRIC_REPRESENTATION_CONTEXT(3)
GLOBAL_UNCERTAINTY_ASSIGNED_CONTEXT((#15430))
GLOBAL_UNIT_ASSIGNED_CONTEXT((#15485,#15487,#15488))
REPRESENTATION_CONTEXT('','3D')
) ;
#15474 = (
GEOMETRIC_REPRESENTATION_CONTEXT(3)
GLOBAL_UNCERTAINTY_ASSIGNED_CONTEXT((#15431))
GLOBAL_UNIT_ASSIGNED_CONTEXT((#15485,#15487,#15488))
REPRESENTATION_CONTEXT('','3D')
) ;
#15475 = (
GEOMETRIC_REPRESENTATION_CONTEXT(3)
GLOBAL_UNCERTAINTY_ASSIGNED_CONTEXT((#15432))
GLOBAL_UNIT_ASSIGNED_CONTEXT((#15485,#15487,#15488))
REPRESENTATION_CONTEXT('','3D')
) ;
#15476 = (
GEOMETRIC_REPRESENTATION_CONTEXT(3)
GLOBAL_UNCERTAINTY_ASSIGNED_CONTEXT((#15433))
GLOBAL_UNIT_ASSIGNED_CONTEXT((#15485,#15487,#15488))
REPRESENTATION_CONTEXT('','3D')
) ;
#15477 = (
GEOMETRIC_REPRESENTATION_CONTEXT(3)
GLOBAL_UNCERTAINTY_ASSIGNED_CONTEXT((#15434))
GLOBAL_UNIT_ASSIGNED_CONTEXT((#15485,#15487,#15488))
REPRESENTATION_CONTEXT('','3D')
) ;
#15478 = (
GEOMETRIC_REPRESENTATION_CONTEXT(3)
GLOBAL_UNCERTAINTY_ASSIGNED_CONTEXT((#15435))
GLOBAL_UNIT_ASSIGNED_CONTEXT((#15485,#15487,#15488))
REPRESENTATION_CONTEXT('','3D')
) ;
#15479 = (
GEOMETRIC_REPRESENTATION_CONTEXT(3)
GLOBAL_UNCERTAINTY_ASSIGNED_CONTEXT((#15436))
GLOBAL_UNIT_ASSIGNED_CONTEXT((#15485,#15487,#15488))
REPRESENTATION_CONTEXT('','3D')
) ;
#15480 = (
GEOMETRIC_REPRESENTATION_CONTEXT(3)
GLOBAL_UNCERTAINTY_ASSIGNED_CONTEXT((#15437))
GLOBAL_UNIT_ASSIGNED_CONTEXT((#15485,#15487,#15488))
REPRESENTATION_CONTEXT('','3D')
) ;
#15481 = (
GEOMETRIC_REPRESENTATION_CONTEXT(3)
GLOBAL_UNCERTAINTY_ASSIGNED_CONTEXT((#15438))
GLOBAL_UNIT_ASSIGNED_CONTEXT((#15485,#15487,#15488))
REPRESENTATION_CONTEXT('','3D')
) ;
#15482 = (
GEOMETRIC_REPRESENTATION_CONTEXT(3)
GLOBAL_UNCERTAINTY_ASSIGNED_CONTEXT((#15439))
GLOBAL_UNIT_ASSIGNED_CONTEXT((#15485,#15487,#15488))
REPRESENTATION_CONTEXT('','3D')
) ;
#15483 = (
GEOMETRIC_REPRESENTATION_CONTEXT(3)
GLOBAL_UNCERTAINTY_ASSIGNED_CONTEXT((#15440))
GLOBAL_UNIT_ASSIGNED_CONTEXT((#15485,#15487,#15488))
REPRESENTATION_CONTEXT('','3D')
) ;
#15484 = (
GEOMETRIC_REPRESENTATION_CONTEXT(3)
GLOBAL_UNCERTAINTY_ASSIGNED_CONTEXT((#15441))
GLOBAL_UNIT_ASSIGNED_CONTEXT((#15485,#15487,#15488))
REPRESENTATION_CONTEXT('','3D')
) ;
#15485 = (
LENGTH_UNIT()
NAMED_UNIT(*)
SI_UNIT(.CENTI.,.METRE.)
) ;
#15486 = (
LENGTH_UNIT()
NAMED_UNIT(*)
SI_UNIT($,.METRE.)
) ;
#15487 = (
NAMED_UNIT(*)
PLANE_ANGLE_UNIT()
SI_UNIT($,.RADIAN.)
) ;
#15488 = (
NAMED_UNIT(*)
SI_UNIT($,.STERADIAN.)
SOLID_ANGLE_UNIT()
) ;
#15489 = SHAPE_DEFINITION_REPRESENTATION(#15531,#15618) ;
#15490 = SHAPE_DEFINITION_REPRESENTATION(#15532,#15619) ;
#15491 = SHAPE_DEFINITION_REPRESENTATION(#15533,#15620) ;
#15492 = SHAPE_DEFINITION_REPRESENTATION(#15534,#15621) ;
#15493 = SHAPE_DEFINITION_REPRESENTATION(#15537,#15622) ;
#15494 = SHAPE_DEFINITION_REPRESENTATION(#15538,#15623) ;
#15495 = SHAPE_DEFINITION_REPRESENTATION(#15539,#15624) ;
#15496 = SHAPE_DEFINITION_REPRESENTATION(#15540,#15625) ;
#15497 = SHAPE_DEFINITION_REPRESENTATION(#15541,#15626) ;
#15498 = SHAPE_DEFINITION_REPRESENTATION(#15546,#15627) ;
#15499 = SHAPE_DEFINITION_REPRESENTATION(#15547,#15628) ;
#15500 = SHAPE_DEFINITION_REPRESENTATION(#15548,#15629) ;
#15501 = SHAPE_DEFINITION_REPRESENTATION(#15549,#15630) ;
#15502 = SHAPE_DEFINITION_REPRESENTATION(#15550,#15631) ;
#15503 = SHAPE_DEFINITION_REPRESENTATION(#15551,#15632) ;
#15504 = SHAPE_DEFINITION_REPRESENTATION(#15552,#15633) ;
#15505 = SHAPE_DEFINITION_REPRESENTATION(#15553,#15634) ;
#15506 = SHAPE_DEFINITION_REPRESENTATION(#15554,#15635) ;
#15507 = SHAPE_DEFINITION_REPRESENTATION(#15555,#15636) ;
#15508 = SHAPE_DEFINITION_REPRESENTATION(#15565,#15637) ;
#15509 = SHAPE_DEFINITION_REPRESENTATION(#15566,#15638) ;
#15510 = SHAPE_DEFINITION_REPRESENTATION(#15567,#15639) ;
#15511 = SHAPE_DEFINITION_REPRESENTATION(#15568,#15640) ;
#15512 = SHAPE_DEFINITION_REPRESENTATION(#15569,#15641) ;
#15513 = SHAPE_DEFINITION_REPRESENTATION(#15570,#15642) ;
#15514 = SHAPE_DEFINITION_REPRESENTATION(#15571,#15643) ;
#15515 = SHAPE_DEFINITION_REPRESENTATION(#15572,#15644) ;
#15516 = SHAPE_DEFINITION_REPRESENTATION(#15573,#15645) ;
#15517 = SHAPE_DEFINITION_REPRESENTATION(#15574,#15646) ;
#15518 = SHAPE_DEFINITION_REPRESENTATION(#15575,#15647) ;
#15519 = SHAPE_DEFINITION_REPRESENTATION(#15576,#15648) ;
#15520 = SHAPE_DEFINITION_REPRESENTATION(#15588,#15649) ;
#15521 = SHAPE_DEFINITION_REPRESENTATION(#15589,#15650) ;
#15522 = SHAPE_DEFINITION_REPRESENTATION(#15590,#15651) ;
#15523 = SHAPE_DEFINITION_REPRESENTATION(#15591,#15652) ;
#15524 = SHAPE_DEFINITION_REPRESENTATION(#15592,#15653) ;
#15525 = SHAPE_DEFINITION_REPRESENTATION(#15593,#15654) ;
#15526 = SHAPE_DEFINITION_REPRESENTATION(#15594,#15655) ;
#15527 = SHAPE_DEFINITION_REPRESENTATION(#15595,#15656) ;
#15528 = SHAPE_DEFINITION_REPRESENTATION(#15605,#15657) ;
#15529 = SHAPE_DEFINITION_REPRESENTATION(#15606,#15658) ;
#15530 = SHAPE_DEFINITION_REPRESENTATION(#15607,#15659) ;
#15531 = PRODUCT_DEFINITION_SHAPE('',$,#15661) ;
#15532 = PRODUCT_DEFINITION_SHAPE('',$,#15662) ;
#15533 = PRODUCT_DEFINITION_SHAPE('',$,#15663) ;
#15534 = PRODUCT_DEFINITION_SHAPE('',$,#15664) ;
#15535 = PRODUCT_DEFINITION_SHAPE($,$,#428) ;
#15536 = PRODUCT_DEFINITION_SHAPE($,$,#429) ;
#15537 = PRODUCT_DEFINITION_SHAPE('',$,#15665) ;
#15538 = PRODUCT_DEFINITION_SHAPE('',$,#15666) ;
#15539 = PRODUCT_DEFINITION_SHAPE('',$,#15667) ;
#15540 = PRODUCT_DEFINITION_SHAPE('',$,#15668) ;
#15541 = PRODUCT_DEFINITION_SHAPE('',$,#15669) ;
#15542 = PRODUCT_DEFINITION_SHAPE($,$,#430) ;
#15543 = PRODUCT_DEFINITION_SHAPE($,$,#431) ;
#15544 = PRODUCT_DEFINITION_SHAPE($,$,#432) ;
#15545 = PRODUCT_DEFINITION_SHAPE($,$,#433) ;
#15546 = PRODUCT_DEFINITION_SHAPE('',$,#15670) ;
#15547 = PRODUCT_DEFINITION_SHAPE('',$,#15671) ;
#15548 = PRODUCT_DEFINITION_SHAPE('',$,#15672) ;
#15549 = PRODUCT_DEFINITION_SHAPE('',$,#15673) ;
#15550 = PRODUCT_DEFINITION_SHAPE('',$,#15674) ;
#15551 = PRODUCT_DEFINITION_SHAPE('',$,#15675) ;
#15552 = PRODUCT_DEFINITION_SHAPE('',$,#15676) ;
#15553 = PRODUCT_DEFINITION_SHAPE('',$,#15677) ;
#15554 = PRODUCT_DEFINITION_SHAPE('',$,#15678) ;
#15555 = PRODUCT_DEFINITION_SHAPE('',$,#15679) ;
#15556 = PRODUCT_DEFINITION_SHAPE($,$,#434) ;
#15557 = PRODUCT_DEFINITION_SHAPE($,$,#435) ;
#15558 = PRODUCT_DEFINITION_SHAPE($,$,#436) ;
#15559 = PRODUCT_DEFINITION_SHAPE($,$,#437) ;
#15560 = PRODUCT_DEFINITION_SHAPE($,$,#438) ;
#15561 = PRODUCT_DEFINITION_SHAPE($,$,#439) ;
#15562 = PRODUCT_DEFINITION_SHAPE($,$,#440) ;
#15563 = PRODUCT_DEFINITION_SHAPE($,$,#441) ;
#15564 = PRODUCT_DEFINITION_SHAPE($,$,#442) ;
#15565 = PRODUCT_DEFINITION_SHAPE('',$,#15680) ;
#15566 = PRODUCT_DEFINITION_SHAPE('',$,#15681) ;
#15567 = PRODUCT_DEFINITION_SHAPE('',$,#15682) ;
#15568 = PRODUCT_DEFINITION_SHAPE('',$,#15683) ;
#15569 = PRODUCT_DEFINITION_SHAPE('',$,#15684) ;
#15570 = PRODUCT_DEFINITION_SHAPE('',$,#15685) ;
#15571 = PRODUCT_DEFINITION_SHAPE('',$,#15686) ;
#15572 = PRODUCT_DEFINITION_SHAPE('',$,#15687) ;
#15573 = PRODUCT_DEFINITION_SHAPE('',$,#15688) ;
#15574 = PRODUCT_DEFINITION_SHAPE('',$,#15689) ;
#15575 = PRODUCT_DEFINITION_SHAPE('',$,#15690) ;
#15576 = PRODUCT_DEFINITION_SHAPE('',$,#15691) ;
#15577 = PRODUCT_DEFINITION_SHAPE($,$,#443) ;
#15578 = PRODUCT_DEFINITION_SHAPE($,$,#444) ;
#15579 = PRODUCT_DEFINITION_SHAPE($,$,#445) ;
#15580 = PRODUCT_DEFINITION_SHAPE($,$,#446) ;
#15581 = PRODUCT_DEFINITION_SHAPE($,$,#447) ;
#15582 = PRODUCT_DEFINITION_SHAPE($,$,#448) ;
#15583 = PRODUCT_DEFINITION_SHAPE($,$,#449) ;
#15584 = PRODUCT_DEFINITION_SHAPE($,$,#450) ;
#15585 = PRODUCT_DEFINITION_SHAPE($,$,#451) ;
#15586 = PRODUCT_DEFINITION_SHAPE($,$,#452) ;
#15587 = PRODUCT_DEFINITION_SHAPE($,$,#453) ;
#15588 = PRODUCT_DEFINITION_SHAPE('',$,#15692) ;
#15589 = PRODUCT_DEFINITION_SHAPE('',$,#15693) ;
#15590 = PRODUCT_DEFINITION_SHAPE('',$,#15694) ;
#15591 = PRODUCT_DEFINITION_SHAPE('',$,#15695) ;
#15592 = PRODUCT_DEFINITION_SHAPE('',$,#15696) ;
#15593 = PRODUCT_DEFINITION_SHAPE('',$,#15697) ;
#15594 = PRODUCT_DEFINITION_SHAPE('',$,#15698) ;
#15595 = PRODUCT_DEFINITION_SHAPE('',$,#15699) ;
#15596 = PRODUCT_DEFINITION_SHAPE($,$,#454) ;
#15597 = PRODUCT_DEFINITION_SHAPE($,$,#455) ;
#15598 = PRODUCT_DEFINITION_SHAPE($,$,#456) ;
#15599 = PRODUCT_DEFINITION_SHAPE($,$,#457) ;
#15600 = PRODUCT_DEFINITION_SHAPE($,$,#458) ;
#15601 = PRODUCT_DEFINITION_SHAPE($,$,#459) ;
#15602 = PRODUCT_DEFINITION_SHAPE($,$,#460) ;
#15603 = PRODUCT_DEFINITION_SHAPE($,$,#461) ;
#15604 = PRODUCT_DEFINITION_SHAPE($,$,#462) ;
#15605 = PRODUCT_DEFINITION_SHAPE('',$,#15700) ;
#15606 = PRODUCT_DEFINITION_SHAPE('',$,#15701) ;
#15607 = PRODUCT_DEFINITION_SHAPE('',$,#15702) ;
#15608 = PRODUCT_DEFINITION_SHAPE($,$,#463) ;
#15609 = PRODUCT_DEFINITION_SHAPE($,$,#464) ;
#15610 = PRODUCT_DEFINITION_SHAPE($,$,#465) ;
#15611 = PRODUCT_DEFINITION_SHAPE($,$,#466) ;
#15612 = PRODUCT_DEFINITION_SHAPE($,$,#467) ;
#15613 = PRODUCT_DEFINITION_SHAPE($,$,#468) ;
#15614 = PRODUCT_DEFINITION_SHAPE($,$,#469) ;
#15615 = PRODUCT_DEFINITION_SHAPE($,$,#470) ;
#15616 = PRODUCT_DEFINITION_SHAPE($,$,#471) ;
#15617 = PRODUCT_DEFINITION_SHAPE($,$,#472) ;
#15618 = SHAPE_REPRESENTATION('',(#8682,#9919,#9920,#9921,#9922,#9923,#9924),
#15442) ;
#15619 = SHAPE_REPRESENTATION('',(#8683,#8796,#8797),#15443) ;
#15620 = SHAPE_REPRESENTATION('',(#8684),#15444) ;
#15621 = SHAPE_REPRESENTATION('',(#8764),#15445) ;
#15622 = SHAPE_REPRESENTATION('',(#8798,#8865,#8866,#8867,#8868),#15446) ;
#15623 = SHAPE_REPRESENTATION('',(#8799),#15447) ;
#15624 = SHAPE_REPRESENTATION('',(#8840),#15448) ;
#15625 = SHAPE_REPRESENTATION('',(#8849),#15449) ;
#15626 = SHAPE_REPRESENTATION('',(#8858),#15450) ;
#15627 = SHAPE_REPRESENTATION('',(#8869,#9001,#9002,#9003,#9004,#9005,#9006,
#9007,#9008,#9009),#15451) ;
#15628 = SHAPE_REPRESENTATION('',(#8870),#15452) ;
#15629 = SHAPE_REPRESENTATION('',(#8883),#15453) ;
#15630 = SHAPE_REPRESENTATION('',(#8893),#15454) ;
#15631 = SHAPE_REPRESENTATION('',(#8899),#15455) ;
#15632 = SHAPE_REPRESENTATION('',(#8932),#15456) ;
#15633 = SHAPE_REPRESENTATION('',(#8967),#15457) ;
#15634 = SHAPE_REPRESENTATION('',(#8976),#15458) ;
#15635 = SHAPE_REPRESENTATION('',(#8989),#15459) ;
#15636 = SHAPE_REPRESENTATION('',(#8995),#15460) ;
#15637 = SHAPE_REPRESENTATION('',(#9010,#9768,#9769,#9770,#9771,#9772,#9773,
#9774,#9775,#9776,#9777,#9778),#15461) ;
#15638 = SHAPE_REPRESENTATION('',(#9011),#15462) ;
#15639 = SHAPE_REPRESENTATION('',(#9034),#15463) ;
#15640 = SHAPE_REPRESENTATION('',(#9044),#15464) ;
#15641 = SHAPE_REPRESENTATION('',(#9319),#15465) ;
#15642 = SHAPE_REPRESENTATION('',(#9333),#15466) ;
#15643 = SHAPE_REPRESENTATION('',(#9349),#15467) ;
#15644 = SHAPE_REPRESENTATION('',(#9514),#15468) ;
#15645 = SHAPE_REPRESENTATION('',(#9525),#15469) ;
#15646 = SHAPE_REPRESENTATION('',(#9536),#15470) ;
#15647 = SHAPE_REPRESENTATION('',(#9542),#15471) ;
#15648 = SHAPE_REPRESENTATION('',(#9548),#15472) ;
#15649 = SHAPE_REPRESENTATION('',(#9779,#9885,#9886,#9887,#9888,#9889,#9890,
#9891,#9892,#9893),#15473) ;
#15650 = SHAPE_REPRESENTATION('',(#9780),#15474) ;
#15651 = SHAPE_REPRESENTATION('',(#9794),#15475) ;
#15652 = SHAPE_REPRESENTATION('',(#9809),#15476) ;
#15653 = SHAPE_REPRESENTATION('',(#9828),#15477) ;
#15654 = SHAPE_REPRESENTATION('',(#9844),#15478) ;
#15655 = SHAPE_REPRESENTATION('',(#9863),#15479) ;
#15656 = SHAPE_REPRESENTATION('',(#9879),#15480) ;
#15657 = SHAPE_REPRESENTATION('',(#9894,#9915,#9916,#9917,#9918),#15481) ;
#15658 = SHAPE_REPRESENTATION('',(#9895),#15482) ;
#15659 = SHAPE_REPRESENTATION('',(#9905),#15483) ;
#15660 = PRODUCT_DEFINITION_CONTEXT('part definition',#15788,'design') ;
#15661 = PRODUCT_DEFINITION('BR-817',
'BR-817',#15703,#15660) ;
#15662 = PRODUCT_DEFINITION('CONTROL_HOUSING_UNIT',
'CONTROL_HOUSING_UNIT',#15704,#15660) ;
#15663 = PRODUCT_DEFINITION('CONTROL_HOUSING_BODY',
'CONTROL_HOUSING_BODY',#15705,#15660) ;
#15664 = PRODUCT_DEFINITION('BASE_STATION_CORD_RETAINER',
'BASE_STATION_CORD_RETAINER',#15706,#15660) ;
#15665 = PRODUCT_DEFINITION('CONNECTOR_UNIT','CONNECTOR_UNIT',#15707,
#15660) ;
#15666 = PRODUCT_DEFINITION('STANDARD_3PIN_STRIX_CONNECTOR_BASE',
'STANDARD_3PIN_STRIX_CONNECTOR_BASE',#15708,#15660) ;
#15667 = PRODUCT_DEFINITION('EARTH_CONTACT_RING',
'EARTH_CONTACT_RING',#15709,#15660) ;
#15668 = PRODUCT_DEFINITION('LIVE_CONTACT_RING','LIVE_CONTACT_RING',
#15710,#15660) ;
#15669 = PRODUCT_DEFINITION('NEUTRAL_CENTRE_PIN',
'NEUTRAL_CENTRE_PIN',#15711,#15660) ;
#15670 = PRODUCT_DEFINITION('THERMAL_SENSING_UNIT',
'THERMAL_SENSING_UNIT',#15712,#15660) ;
#15671 = PRODUCT_DEFINITION('STEAM_DISC_HOLDER_CUP',
'STEAM_DISC_HOLDER_CUP',#15713,#15660) ;
#15672 = PRODUCT_DEFINITION('BIMETALLIC_THERMOSTATIC_DISC_UNIT',
'BIMETALLIC_THERMOSTATIC_DISC_UNIT',#15714,#15660) ;
#15673 = PRODUCT_DEFINITION('STEAM_DISC_PUSH_ROD',
'STEAM_DISC_PUSH_ROD',#15715,#15660) ;
#15674 = PRODUCT_DEFINITION('STEAM_PORT_DEFLECTOR_CAP',
'STEAM_PORT_DEFLECTOR_CAP',#15716,#15660) ;
#15675 = PRODUCT_DEFINITION('INTERNAL_STEAM_TUBE_CONDUIT',
'INTERNAL_STEAM_TUBE_CONDUIT',#15717,#15660) ;
#15676 = PRODUCT_DEFINITION('STEAM_SEAL_GROMMET',
'STEAM_SEAL_GROMMET',#15718,#15660) ;
#15677 = PRODUCT_DEFINITION('DRY_BOIL_DISC_HOLDER',
'DRY_BOIL_DISC_HOLDER',#15719,#15660) ;
#15678 = PRODUCT_DEFINITION('DRY_BOIL_BIMETAL_DISC',
'DRY_BOIL_BIMETAL_DISC',#15720,#15660) ;
#15679 = PRODUCT_DEFINITION('DRY_BOIL_PUSH_ROD','DRY_BOIL_PUSH_ROD',
#15721,#15660) ;
#15680 = PRODUCT_DEFINITION('SWITCH_MECHANISM_UNIT',
'SWITCH_MECHANISM_UNIT',#15722,#15660) ;
#15681 = PRODUCT_DEFINITION('AUTO_OFF_LATCH_TRIP_LEVER',
'AUTO_OFF_LATCH_TRIP_LEVER',#15723,#15660) ;
#15682 = PRODUCT_DEFINITION('TRIP_LEVER_PIVOT_PIN',
'TRIP_LEVER_PIVOT_PIN',#15724,#15660) ;
#15683 = PRODUCT_DEFINITION('TRIP_LEVER_RETURN_SPRING',
'TRIP_LEVER_RETURN_SPRING',#15725,#15660) ;
#15684 = PRODUCT_DEFINITION('PUSH_BUTTON_STEM','PUSH_BUTTON_STEM',
#15726,#15660) ;
#15685 = PRODUCT_DEFINITION('PUSH_BUTTON_CAP','PUSH_BUTTON_CAP',#15727,
#15660) ;
#15686 = PRODUCT_DEFINITION('BUTTON_RETURN_SPRING',
'BUTTON_RETURN_SPRING',#15728,#15660) ;
#15687 = PRODUCT_DEFINITION('MOVING_CONTACT_ARM',
'MOVING_CONTACT_ARM',#15729,#15660) ;
#15688 = PRODUCT_DEFINITION('CONTACT_ANCHOR_POST',
'CONTACT_ANCHOR_POST',#15730,#15660) ;
#15689 = PRODUCT_DEFINITION('FIXED_CONTACT_POST',
'FIXED_CONTACT_POST',#15731,#15660) ;
#15690 = PRODUCT_DEFINITION('CONTACT_RIVET_SILVER',
'CONTACT_RIVET_SILVER',#15732,#15660) ;
#15691 = PRODUCT_DEFINITION('CONTACT_PRESSURE_SPRING',
'CONTACT_PRESSURE_SPRING',#15733,#15660) ;
#15692 = PRODUCT_DEFINITION('ELECTRICAL_UNIT','ELECTRICAL_UNIT',#15734,
#15660) ;
#15693 = PRODUCT_DEFINITION('ELECTRICAL_TERMINAL_CONTACT_PIN',
'ELECTRICAL_TERMINAL_CONTACT_PIN',#15735,#15660) ;
#15694 = PRODUCT_DEFINITION('INDICATOR_LED_LIGHT_HOUSING',
'INDICATOR_LED_LIGHT_HOUSING',#15736,#15660) ;
#15695 = PRODUCT_DEFINITION('LED_LAMP','LED_LAMP',#15737,#15660) ;
#15696 = PRODUCT_DEFINITION('LED_SERIES_RESISTOR',
'LED_SERIES_RESISTOR',#15738,#15660) ;
#15697 = PRODUCT_DEFINITION('THERMAL_FUSE_CUTOUT_BLOCK',
'THERMAL_FUSE_CUTOUT_BLOCK',#15739,#15660) ;
#15698 = PRODUCT_DEFINITION('THERMAL_FUSE_ELEMENT',
'THERMAL_FUSE_ELEMENT',#15740,#15660) ;
#15699 = PRODUCT_DEFINITION('MAINS_CORD_STUB','MAINS_CORD_STUB',#15741,
#15660) ;
#15700 = PRODUCT_DEFINITION('FASTENERS','FASTENERS',#15742,
#15660) ;
#15701 = PRODUCT_DEFINITION('RETAINER_SCREW_M3x8',
'RETAINER_SCREW_M3x8',#15743,#15660) ;
#15702 = PRODUCT_DEFINITION('MOUNTING_SCREW_M3x8',
'MOUNTING_SCREW_M3x8',#15744,#15660) ;
#15703 = PRODUCT_DEFINITION_FORMATION('',$,#15790) ;
#15704 = PRODUCT_DEFINITION_FORMATION('',$,#15791) ;
#15705 = PRODUCT_DEFINITION_FORMATION('',$,#15792) ;
#15706 = PRODUCT_DEFINITION_FORMATION('',$,#15793) ;
#15707 = PRODUCT_DEFINITION_FORMATION('',$,#15794) ;
#15708 = PRODUCT_DEFINITION_FORMATION('',$,#15795) ;
#15709 = PRODUCT_DEFINITION_FORMATION('',$,#15796) ;
#15710 = PRODUCT_DEFINITION_FORMATION('',$,#15797) ;
#15711 = PRODUCT_DEFINITION_FORMATION('',$,#15798) ;
#15712 = PRODUCT_DEFINITION_FORMATION('',$,#15799) ;
#15713 = PRODUCT_DEFINITION_FORMATION('',$,#15800) ;
#15714 = PRODUCT_DEFINITION_FORMATION('',$,#15801) ;
#15715 = PRODUCT_DEFINITION_FORMATION('',$,#15802) ;
#15716 = PRODUCT_DEFINITION_FORMATION('',$,#15803) ;
#15717 = PRODUCT_DEFINITION_FORMATION('',$,#15804) ;
#15718 = PRODUCT_DEFINITION_FORMATION('',$,#15805) ;
#15719 = PRODUCT_DEFINITION_FORMATION('',$,#15806) ;
#15720 = PRODUCT_DEFINITION_FORMATION('',$,#15807) ;
#15721 = PRODUCT_DEFINITION_FORMATION('',$,#15808) ;
#15722 = PRODUCT_DEFINITION_FORMATION('',$,#15809) ;
#15723 = PRODUCT_DEFINITION_FORMATION('',$,#15810) ;
#15724 = PRODUCT_DEFINITION_FORMATION('',$,#15811) ;
#15725 = PRODUCT_DEFINITION_FORMATION('',$,#15812) ;
#15726 = PRODUCT_DEFINITION_FORMATION('',$,#15813) ;
#15727 = PRODUCT_DEFINITION_FORMATION('',$,#15814) ;
#15728 = PRODUCT_DEFINITION_FORMATION('',$,#15815) ;
#15729 = PRODUCT_DEFINITION_FORMATION('',$,#15816) ;
#15730 = PRODUCT_DEFINITION_FORMATION('',$,#15817) ;
#15731 = PRODUCT_DEFINITION_FORMATION('',$,#15818) ;
#15732 = PRODUCT_DEFINITION_FORMATION('',$,#15819) ;
#15733 = PRODUCT_DEFINITION_FORMATION('',$,#15820) ;
#15734 = PRODUCT_DEFINITION_FORMATION('',$,#15821) ;
#15735 = PRODUCT_DEFINITION_FORMATION('',$,#15822) ;
#15736 = PRODUCT_DEFINITION_FORMATION('',$,#15823) ;
#15737 = PRODUCT_DEFINITION_FORMATION('',$,#15824) ;
#15738 = PRODUCT_DEFINITION_FORMATION('',$,#15825) ;
#15739 = PRODUCT_DEFINITION_FORMATION('',$,#15826) ;
#15740 = PRODUCT_DEFINITION_FORMATION('',$,#15827) ;
#15741 = PRODUCT_DEFINITION_FORMATION('',$,#15828) ;
#15742 = PRODUCT_DEFINITION_FORMATION('',$,#15829) ;
#15743 = PRODUCT_DEFINITION_FORMATION('',$,#15830) ;
#15744 = PRODUCT_DEFINITION_FORMATION('',$,#15831) ;
#15745 = PRODUCT_RELATED_PRODUCT_CATEGORY('BR-817',
'BR-817',(#15790)) ;
#15746 = PRODUCT_RELATED_PRODUCT_CATEGORY('CONTROL_HOUSING_UNIT',
'CONTROL_HOUSING_UNIT',(#15791)) ;
#15747 = PRODUCT_RELATED_PRODUCT_CATEGORY('CONTROL_HOUSING_BODY',
'CONTROL_HOUSING_BODY',(#15792)) ;
#15748 = PRODUCT_RELATED_PRODUCT_CATEGORY('BASE_STATION_CORD_RETAINER',
'BASE_STATION_CORD_RETAINER',(#15793)) ;
#15749 = PRODUCT_RELATED_PRODUCT_CATEGORY('CONNECTOR_UNIT',
'CONNECTOR_UNIT',(#15794)) ;
#15750 = PRODUCT_RELATED_PRODUCT_CATEGORY(
'STANDARD_3PIN_STRIX_CONNECTOR_BASE',
'STANDARD_3PIN_STRIX_CONNECTOR_BASE',(#15795)) ;
#15751 = PRODUCT_RELATED_PRODUCT_CATEGORY('EARTH_CONTACT_RING',
'EARTH_CONTACT_RING',(#15796)) ;
#15752 = PRODUCT_RELATED_PRODUCT_CATEGORY('LIVE_CONTACT_RING',
'LIVE_CONTACT_RING',(#15797)) ;
#15753 = PRODUCT_RELATED_PRODUCT_CATEGORY('NEUTRAL_CENTRE_PIN',
'NEUTRAL_CENTRE_PIN',(#15798)) ;
#15754 = PRODUCT_RELATED_PRODUCT_CATEGORY('THERMAL_SENSING_UNIT',
'THERMAL_SENSING_UNIT',(#15799)) ;
#15755 = PRODUCT_RELATED_PRODUCT_CATEGORY('STEAM_DISC_HOLDER_CUP',
'STEAM_DISC_HOLDER_CUP',(#15800)) ;
#15756 = PRODUCT_RELATED_PRODUCT_CATEGORY(
'BIMETALLIC_THERMOSTATIC_DISC_UNIT','BIMETALLIC_THERMOSTATIC_DISC_UNIT',
(#15801)) ;
#15757 = PRODUCT_RELATED_PRODUCT_CATEGORY('STEAM_DISC_PUSH_ROD',
'STEAM_DISC_PUSH_ROD',(#15802)) ;
#15758 = PRODUCT_RELATED_PRODUCT_CATEGORY('STEAM_PORT_DEFLECTOR_CAP',
'STEAM_PORT_DEFLECTOR_CAP',(#15803)) ;
#15759 = PRODUCT_RELATED_PRODUCT_CATEGORY('INTERNAL_STEAM_TUBE_CONDUIT',
'INTERNAL_STEAM_TUBE_CONDUIT',(#15804)) ;
#15760 = PRODUCT_RELATED_PRODUCT_CATEGORY('STEAM_SEAL_GROMMET',
'STEAM_SEAL_GROMMET',(#15805)) ;
#15761 = PRODUCT_RELATED_PRODUCT_CATEGORY('DRY_BOIL_DISC_HOLDER',
'DRY_BOIL_DISC_HOLDER',(#15806)) ;
#15762 = PRODUCT_RELATED_PRODUCT_CATEGORY('DRY_BOIL_BIMETAL_DISC',
'DRY_BOIL_BIMETAL_DISC',(#15807)) ;
#15763 = PRODUCT_RELATED_PRODUCT_CATEGORY('DRY_BOIL_PUSH_ROD',
'DRY_BOIL_PUSH_ROD',(#15808)) ;
#15764 = PRODUCT_RELATED_PRODUCT_CATEGORY('SWITCH_MECHANISM_UNIT',
'SWITCH_MECHANISM_UNIT',(#15809)) ;
#15765 = PRODUCT_RELATED_PRODUCT_CATEGORY('AUTO_OFF_LATCH_TRIP_LEVER',
'AUTO_OFF_LATCH_TRIP_LEVER',(#15810)) ;
#15766 = PRODUCT_RELATED_PRODUCT_CATEGORY('TRIP_LEVER_PIVOT_PIN',
'TRIP_LEVER_PIVOT_PIN',(#15811)) ;
#15767 = PRODUCT_RELATED_PRODUCT_CATEGORY('TRIP_LEVER_RETURN_SPRING',
'TRIP_LEVER_RETURN_SPRING',(#15812)) ;
#15768 = PRODUCT_RELATED_PRODUCT_CATEGORY('PUSH_BUTTON_STEM',
'PUSH_BUTTON_STEM',(#15813)) ;
#15769 = PRODUCT_RELATED_PRODUCT_CATEGORY('PUSH_BUTTON_CAP',
'PUSH_BUTTON_CAP',(#15814)) ;
#15770 = PRODUCT_RELATED_PRODUCT_CATEGORY('BUTTON_RETURN_SPRING',
'BUTTON_RETURN_SPRING',(#15815)) ;
#15771 = PRODUCT_RELATED_PRODUCT_CATEGORY('MOVING_CONTACT_ARM',
'MOVING_CONTACT_ARM',(#15816)) ;
#15772 = PRODUCT_RELATED_PRODUCT_CATEGORY('CONTACT_ANCHOR_POST',
'CONTACT_ANCHOR_POST',(#15817)) ;
#15773 = PRODUCT_RELATED_PRODUCT_CATEGORY('FIXED_CONTACT_POST',
'FIXED_CONTACT_POST',(#15818)) ;
#15774 = PRODUCT_RELATED_PRODUCT_CATEGORY('CONTACT_RIVET_SILVER',
'CONTACT_RIVET_SILVER',(#15819)) ;
#15775 = PRODUCT_RELATED_PRODUCT_CATEGORY('CONTACT_PRESSURE_SPRING',
'CONTACT_PRESSURE_SPRING',(#15820)) ;
#15776 = PRODUCT_RELATED_PRODUCT_CATEGORY('ELECTRICAL_UNIT',
'ELECTRICAL_UNIT',(#15821)) ;
#15777 = PRODUCT_RELATED_PRODUCT_CATEGORY(
'ELECTRICAL_TERMINAL_CONTACT_PIN','ELECTRICAL_TERMINAL_CONTACT_PIN',(#15822)) ;
#15778 = PRODUCT_RELATED_PRODUCT_CATEGORY('INDICATOR_LED_LIGHT_HOUSING',
'INDICATOR_LED_LIGHT_HOUSING',(#15823)) ;
#15779 = PRODUCT_RELATED_PRODUCT_CATEGORY('LED_LAMP','LED_LAMP',(#15824)) ;
#15780 = PRODUCT_RELATED_PRODUCT_CATEGORY('LED_SERIES_RESISTOR',
'LED_SERIES_RESISTOR',(#15825)) ;
#15781 = PRODUCT_RELATED_PRODUCT_CATEGORY('THERMAL_FUSE_CUTOUT_BLOCK',
'THERMAL_FUSE_CUTOUT_BLOCK',(#15826)) ;
#15782 = PRODUCT_RELATED_PRODUCT_CATEGORY('THERMAL_FUSE_ELEMENT',
'THERMAL_FUSE_ELEMENT',(#15827)) ;
#15783 = PRODUCT_RELATED_PRODUCT_CATEGORY('MAINS_CORD_STUB',
'MAINS_CORD_STUB',(#15828)) ;
#15784 = PRODUCT_RELATED_PRODUCT_CATEGORY('FASTENERS','FASTENERS',(#15829)) ;
#15785 = PRODUCT_RELATED_PRODUCT_CATEGORY('RETAINER_SCREW_M3x8',
'RETAINER_SCREW_M3x8',(#15830)) ;
#15786 = PRODUCT_RELATED_PRODUCT_CATEGORY('MOUNTING_SCREW_M3x8',
'MOUNTING_SCREW_M3x8',(#15831)) ;
#15787 = APPLICATION_PROTOCOL_DEFINITION('international standard',
'automotive_design',2009,#15788) ;
#15788 = APPLICATION_CONTEXT(
'Core Data for Automotive Mechanical Design Process') ;
#15789 = PRODUCT_CONTEXT('part definition',#15788,'mechanical') ;
#15790 = PRODUCT('BR-817','BR-817',
$,(#15789)) ;
#15791 = PRODUCT('CONTROL_HOUSING_UNIT','CONTROL_HOUSING_UNIT',$,(#15789)) ;
#15792 = PRODUCT('CONTROL_HOUSING_BODY','CONTROL_HOUSING_BODY',$,(#15789)) ;
#15793 = PRODUCT('BASE_STATION_CORD_RETAINER','BASE_STATION_CORD_RETAINER',$,
(#15789)) ;
#15794 = PRODUCT('CONNECTOR_UNIT','CONNECTOR_UNIT',$,(#15789)) ;
#15795 = PRODUCT('STANDARD_3PIN_STRIX_CONNECTOR_BASE',
'STANDARD_3PIN_STRIX_CONNECTOR_BASE',$,(#15789)) ;
#15796 = PRODUCT('EARTH_CONTACT_RING','EARTH_CONTACT_RING',$,(#15789)) ;
#15797 = PRODUCT('LIVE_CONTACT_RING','LIVE_CONTACT_RING',$,(#15789)) ;
#15798 = PRODUCT('NEUTRAL_CENTRE_PIN','NEUTRAL_CENTRE_PIN',$,(#15789)) ;
#15799 = PRODUCT('THERMAL_SENSING_UNIT','THERMAL_SENSING_UNIT',$,(#15789)) ;
#15800 = PRODUCT('STEAM_DISC_HOLDER_CUP','STEAM_DISC_HOLDER_CUP',$,(#15789)) ;
#15801 = PRODUCT('BIMETALLIC_THERMOSTATIC_DISC_UNIT',
'BIMETALLIC_THERMOSTATIC_DISC_UNIT',$,(#15789)) ;
#15802 = PRODUCT('STEAM_DISC_PUSH_ROD','STEAM_DISC_PUSH_ROD',$,(#15789)) ;
#15803 = PRODUCT('STEAM_PORT_DEFLECTOR_CAP','STEAM_PORT_DEFLECTOR_CAP',$,(#15789)) ;
#15804 = PRODUCT('INTERNAL_STEAM_TUBE_CONDUIT','INTERNAL_STEAM_TUBE_CONDUIT',
$,(#15789)) ;
#15805 = PRODUCT('STEAM_SEAL_GROMMET','STEAM_SEAL_GROMMET',$,(#15789)) ;
#15806 = PRODUCT('DRY_BOIL_DISC_HOLDER','DRY_BOIL_DISC_HOLDER',$,(#15789)) ;
#15807 = PRODUCT('DRY_BOIL_BIMETAL_DISC','DRY_BOIL_BIMETAL_DISC',$,(#15789)) ;
#15808 = PRODUCT('DRY_BOIL_PUSH_ROD','DRY_BOIL_PUSH_ROD',$,(#15789)) ;
#15809 = PRODUCT('SWITCH_MECHANISM_UNIT','SWITCH_MECHANISM_UNIT',$,(#15789)) ;
#15810 = PRODUCT('AUTO_OFF_LATCH_TRIP_LEVER','AUTO_OFF_LATCH_TRIP_LEVER',$,
(#15789)) ;
#15811 = PRODUCT('TRIP_LEVER_PIVOT_PIN','TRIP_LEVER_PIVOT_PIN',$,(#15789)) ;
#15812 = PRODUCT('TRIP_LEVER_RETURN_SPRING','TRIP_LEVER_RETURN_SPRING',$,(#15789)) ;
#15813 = PRODUCT('PUSH_BUTTON_STEM','PUSH_BUTTON_STEM',$,(#15789)) ;
#15814 = PRODUCT('PUSH_BUTTON_CAP','PUSH_BUTTON_CAP',$,(#15789)) ;
#15815 = PRODUCT('BUTTON_RETURN_SPRING','BUTTON_RETURN_SPRING',$,(#15789)) ;
#15816 = PRODUCT('MOVING_CONTACT_ARM','MOVING_CONTACT_ARM',$,(#15789)) ;
#15817 = PRODUCT('CONTACT_ANCHOR_POST','CONTACT_ANCHOR_POST',$,(#15789)) ;
#15818 = PRODUCT('FIXED_CONTACT_POST','FIXED_CONTACT_POST',$,(#15789)) ;
#15819 = PRODUCT('CONTACT_RIVET_SILVER','CONTACT_RIVET_SILVER',$,(#15789)) ;
#15820 = PRODUCT('CONTACT_PRESSURE_SPRING','CONTACT_PRESSURE_SPRING',$,(#15789)) ;
#15821 = PRODUCT('ELECTRICAL_UNIT','ELECTRICAL_UNIT',$,(#15789)) ;
#15822 = PRODUCT('ELECTRICAL_TERMINAL_CONTACT_PIN',
'ELECTRICAL_TERMINAL_CONTACT_PIN',$,(#15789)) ;
#15823 = PRODUCT('INDICATOR_LED_LIGHT_HOUSING','INDICATOR_LED_LIGHT_HOUSING',
$,(#15789)) ;
#15824 = PRODUCT('LED_LAMP','LED_LAMP',$,(#15789)) ;
#15825 = PRODUCT('LED_SERIES_RESISTOR','LED_SERIES_RESISTOR',$,(#15789)) ;
#15826 = PRODUCT('THERMAL_FUSE_CUTOUT_BLOCK','THERMAL_FUSE_CUTOUT_BLOCK',$,
(#15789)) ;
#15827 = PRODUCT('THERMAL_FUSE_ELEMENT','THERMAL_FUSE_ELEMENT',$,(#15789)) ;
#15828 = PRODUCT('MAINS_CORD_STUB','MAINS_CORD_STUB',$,(#15789)) ;
#15829 = PRODUCT('FASTENERS','FASTENERS',$,(#15789)) ;
#15830 = PRODUCT('RETAINER_SCREW_M3x8','RETAINER_SCREW_M3x8',$,(#15789)) ;
#15831 = PRODUCT('MOUNTING_SCREW_M3x8','MOUNTING_SCREW_M3x8',$,(#15789)) ;
#15832 = PRESENTATION_STYLE_ASSIGNMENT((#15844)) ;
#15833 = PRESENTATION_STYLE_ASSIGNMENT((#15845)) ;
#15834 = PRESENTATION_STYLE_ASSIGNMENT((#15846)) ;
#15835 = PRESENTATION_STYLE_ASSIGNMENT((#15847)) ;
#15836 = PRESENTATION_STYLE_ASSIGNMENT((#15848)) ;
#15837 = PRESENTATION_STYLE_ASSIGNMENT((#15849)) ;
#15838 = PRESENTATION_STYLE_ASSIGNMENT((#15850)) ;
#15839 = PRESENTATION_STYLE_ASSIGNMENT((#15851)) ;
#15840 = PRESENTATION_STYLE_ASSIGNMENT((#15852)) ;
#15841 = PRESENTATION_STYLE_ASSIGNMENT((#15853)) ;
#15842 = PRESENTATION_STYLE_ASSIGNMENT((#15854)) ;
#15843 = PRESENTATION_STYLE_ASSIGNMENT((#15855)) ;
#15844 = SURFACE_STYLE_USAGE(.BOTH.,#15856) ;
#15845 = SURFACE_STYLE_USAGE(.BOTH.,#15857) ;
#15846 = SURFACE_STYLE_USAGE(.BOTH.,#15858) ;
#15847 = SURFACE_STYLE_USAGE(.BOTH.,#15859) ;
#15848 = SURFACE_STYLE_USAGE(.BOTH.,#15860) ;
#15849 = SURFACE_STYLE_USAGE(.BOTH.,#15861) ;
#15850 = SURFACE_STYLE_USAGE(.BOTH.,#15862) ;
#15851 = SURFACE_STYLE_USAGE(.BOTH.,#15863) ;
#15852 = SURFACE_STYLE_USAGE(.BOTH.,#15864) ;
#15853 = SURFACE_STYLE_USAGE(.BOTH.,#15865) ;
#15854 = SURFACE_STYLE_USAGE(.BOTH.,#15866) ;
#15855 = SURFACE_STYLE_USAGE(.BOTH.,#15867) ;
#15856 = SURFACE_SIDE_STYLE('',(#15868)) ;
#15857 = SURFACE_SIDE_STYLE('',(#15869)) ;
#15858 = SURFACE_SIDE_STYLE('',(#15870)) ;
#15859 = SURFACE_SIDE_STYLE('',(#15871)) ;
#15860 = SURFACE_SIDE_STYLE('',(#15872)) ;
#15861 = SURFACE_SIDE_STYLE('',(#15873)) ;
#15862 = SURFACE_SIDE_STYLE('',(#15874)) ;
#15863 = SURFACE_SIDE_STYLE('',(#15875)) ;
#15864 = SURFACE_SIDE_STYLE('',(#15876)) ;
#15865 = SURFACE_SIDE_STYLE('',(#15877)) ;
#15866 = SURFACE_SIDE_STYLE('',(#15878)) ;
#15867 = SURFACE_SIDE_STYLE('',(#15879)) ;
#15868 = SURFACE_STYLE_FILL_AREA(#15880) ;
#15869 = SURFACE_STYLE_FILL_AREA(#15881) ;
#15870 = SURFACE_STYLE_FILL_AREA(#15882) ;
#15871 = SURFACE_STYLE_FILL_AREA(#15883) ;
#15872 = SURFACE_STYLE_FILL_AREA(#15884) ;
#15873 = SURFACE_STYLE_FILL_AREA(#15885) ;
#15874 = SURFACE_STYLE_FILL_AREA(#15886) ;
#15875 = SURFACE_STYLE_FILL_AREA(#15887) ;
#15876 = SURFACE_STYLE_FILL_AREA(#15888) ;
#15877 = SURFACE_STYLE_FILL_AREA(#15889) ;
#15878 = SURFACE_STYLE_FILL_AREA(#15890) ;
#15879 = SURFACE_STYLE_FILL_AREA(#15891) ;
#15880 = FILL_AREA_STYLE('Steel - Satin',(#15892)) ;
#15881 = FILL_AREA_STYLE('Nylon 6-6 (White)',(#15893)) ;
#15882 = FILL_AREA_STYLE('Brass - Polished',(#15894)) ;
#15883 = FILL_AREA_STYLE('Stainless Steel - Satin',(#15895)) ;
#15884 = FILL_AREA_STYLE('Surface - Matte',(#15896)) ;
#15885 = FILL_AREA_STYLE('Silicone (White)',(#15897)) ;
#15886 = FILL_AREA_STYLE('ABS (White)',(#15898)) ;
#15887 = FILL_AREA_STYLE('Nickel - Polished',(#15899)) ;
#15888 = FILL_AREA_STYLE('Polycarbonate (Clear)',(#15900)) ;
#15889 = FILL_AREA_STYLE('Plastic - Glossy (Grey)',(#15901)) ;
#15890 = FILL_AREA_STYLE('Copper - Polished',(#15902)) ;
#15891 = FILL_AREA_STYLE('Rubber - Soft',(#15903)) ;
#15892 = FILL_AREA_STYLE_COLOUR('Steel - Satin',#15904) ;
#15893 = FILL_AREA_STYLE_COLOUR('Nylon 6-6 (White)',#15905) ;
#15894 = FILL_AREA_STYLE_COLOUR('Brass - Polished',#15906) ;
#15895 = FILL_AREA_STYLE_COLOUR('Stainless Steel - Satin',#15907) ;
#15896 = FILL_AREA_STYLE_COLOUR('Surface - Matte',#15908) ;
#15897 = FILL_AREA_STYLE_COLOUR('Silicone (White)',#15909) ;
#15898 = FILL_AREA_STYLE_COLOUR('ABS (White)',#15910) ;
#15899 = FILL_AREA_STYLE_COLOUR('Nickel - Polished',#15911) ;
#15900 = FILL_AREA_STYLE_COLOUR('Polycarbonate (Clear)',#15912) ;
#15901 = FILL_AREA_STYLE_COLOUR('Plastic - Glossy (Grey)',#15913) ;
#15902 = FILL_AREA_STYLE_COLOUR('Copper - Polished',#15914) ;
#15903 = FILL_AREA_STYLE_COLOUR('Rubber - Soft',#15915) ;
#15904 = COLOUR_RGB('Steel - Satin', 0.72549020, 0.75294118, 0.79215686) ;
#15905 = COLOUR_RGB('Nylon 6-6 (White)', 0.31764706, 0.68627451, 0.89019608) ;
#15906 = COLOUR_RGB('Brass - Polished', 0.08235294, 0.09019608, 0.10196078) ;
#15907 = COLOUR_RGB('Stainless Steel - Satin', 0.40784314, 0.44705882, 0.49803922) ;
#15908 = COLOUR_RGB('Surface - Matte', 0.08235294, 0.09019608, 0.10196078) ;
#15909 = COLOUR_RGB('Silicone (White)', 0.09019608, 0.27058824, 0.51372549) ;
#15910 = COLOUR_RGB('ABS (White)', 0.31764706, 0.68627451, 0.89019608) ;
#15911 = COLOUR_RGB('Nickel - Polished', 0.31764706, 0.68627451, 0.89019608) ;
#15912 = COLOUR_RGB('Polycarbonate (Clear)', 0.08235294, 0.09019608, 0.10196078) ;
#15913 = COLOUR_RGB('Plastic - Glossy (Grey)', 0.09019608, 0.27058824, 0.51372549) ;
#15914 = COLOUR_RGB('Copper - Polished', 0.66274510, 0.83137255, 0.94901961) ;
#15915 = COLOUR_RGB('Rubber - Soft', 0.72549020, 0.75294118, 0.79215686) ;
ENDSEC;
END-ISO-10303-21;
